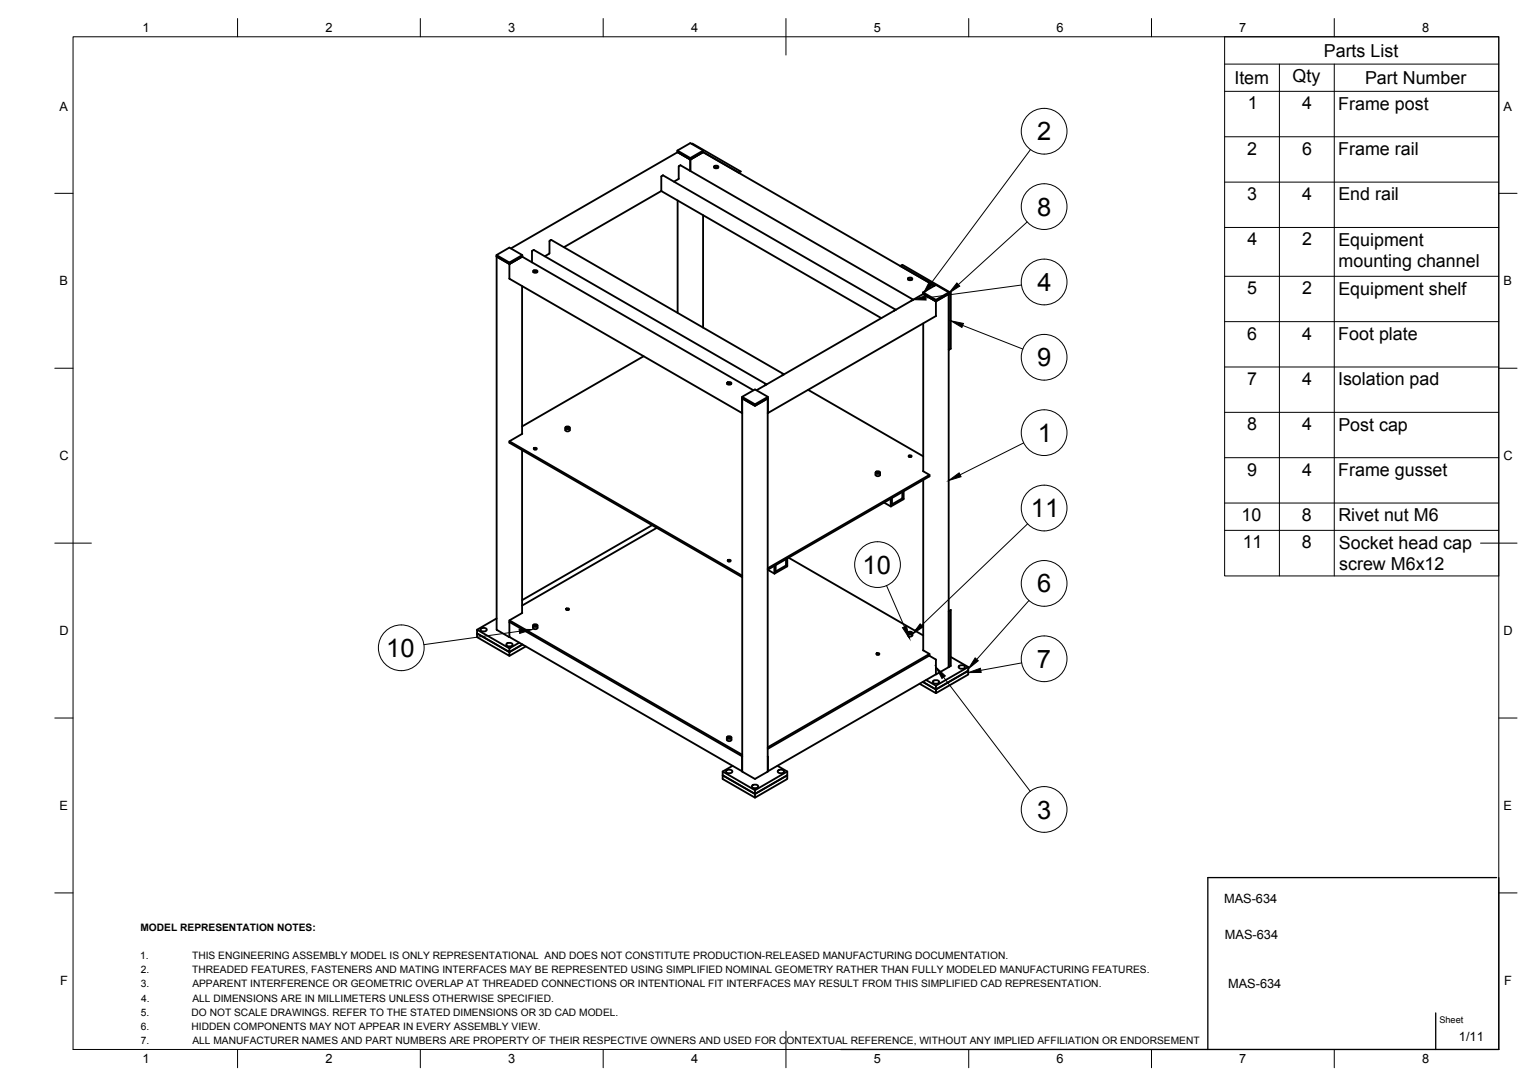
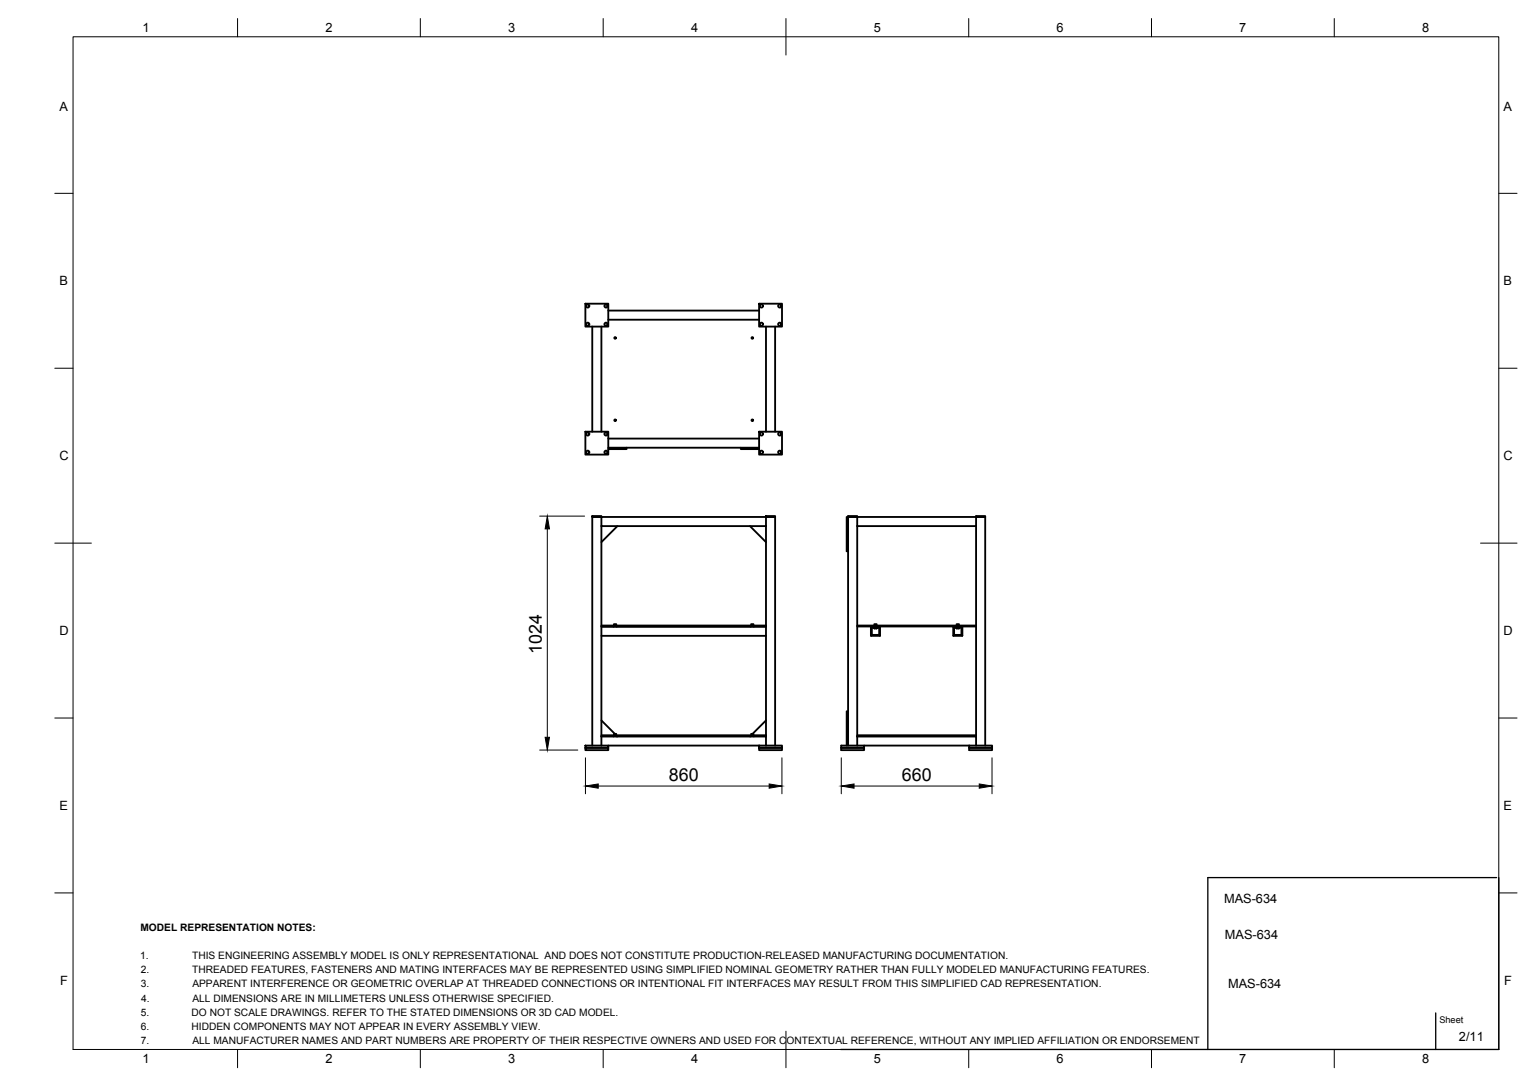
ISO-10303-21;
HEADER;
/* Generated by software containing ST-Developer
 * from STEP Tools, Inc. (www.steptools.com) 
 */

FILE_DESCRIPTION(
/* description */ ('Independent AHU equipment rack. Nominal800x600 frame on1000long40squa
re aluminum posts; two removable notched shelves; welded perimeter/cro
ss rails and rear gussets; two mounting channels; four isolation pads 
and anchor-ready feet. Imported native extrusion library retained and 
cut-length parameters customized per family. Shelf hardware uses model
ed M6 rivet nuts and screws. Weld design, floor anchors and load ratin
g require engineering selection.'),
/* implementation_level */ '2;1');

FILE_NAME(
/* name */ 'MAS-634.step',
/* time_stamp */ '2026-11-07T19:04:45-08:00',
/* author */ (''),
/* organization */ (''),
/* preprocessor_version */ 'ST-DEVELOPER v20.2',
/* originating_system */ 'Autodesk Translation Framework v15.17.0.0',
/* authorisation */ '');

FILE_SCHEMA (('AUTOMOTIVE_DESIGN { 1 0 10303 214 3 1 1 }'));
ENDSEC;

DATA;
#10=MECHANICAL_DESIGN_GEOMETRIC_PRESENTATION_REPRESENTATION('',(#335,#336,
#337,#338,#339,#340,#341,#342,#343,#344,#345),#9777);
#11=ITEM_DEFINED_TRANSFORMATION($,$,#3974,#4302);
#12=ITEM_DEFINED_TRANSFORMATION($,$,#4009,#4303);
#13=ITEM_DEFINED_TRANSFORMATION($,$,#3974,#4304);
#14=ITEM_DEFINED_TRANSFORMATION($,$,#3974,#4305);
#15=ITEM_DEFINED_TRANSFORMATION($,$,#3974,#4306);
#16=ITEM_DEFINED_TRANSFORMATION($,$,#4050,#4307);
#17=ITEM_DEFINED_TRANSFORMATION($,$,#4009,#4308);
#18=ITEM_DEFINED_TRANSFORMATION($,$,#4009,#4309);
#19=ITEM_DEFINED_TRANSFORMATION($,$,#4009,#4310);
#20=ITEM_DEFINED_TRANSFORMATION($,$,#4009,#4311);
#21=ITEM_DEFINED_TRANSFORMATION($,$,#4009,#4312);
#22=ITEM_DEFINED_TRANSFORMATION($,$,#4085,#4313);
#23=ITEM_DEFINED_TRANSFORMATION($,$,#4050,#4314);
#24=ITEM_DEFINED_TRANSFORMATION($,$,#4050,#4315);
#25=ITEM_DEFINED_TRANSFORMATION($,$,#4050,#4316);
#26=ITEM_DEFINED_TRANSFORMATION($,$,#4126,#4317);
#27=ITEM_DEFINED_TRANSFORMATION($,$,#4165,#4318);
#28=ITEM_DEFINED_TRANSFORMATION($,$,#4184,#4319);
#29=ITEM_DEFINED_TRANSFORMATION($,$,#4203,#4320);
#30=ITEM_DEFINED_TRANSFORMATION($,$,#4210,#4321);
#31=ITEM_DEFINED_TRANSFORMATION($,$,#4216,#4322);
#32=ITEM_DEFINED_TRANSFORMATION($,$,#4258,#4323);
#33=ITEM_DEFINED_TRANSFORMATION($,$,#4085,#4324);
#34=ITEM_DEFINED_TRANSFORMATION($,$,#4126,#4325);
#35=ITEM_DEFINED_TRANSFORMATION($,$,#4165,#4326);
#36=ITEM_DEFINED_TRANSFORMATION($,$,#4165,#4327);
#37=ITEM_DEFINED_TRANSFORMATION($,$,#4165,#4328);
#38=ITEM_DEFINED_TRANSFORMATION($,$,#4184,#4329);
#39=ITEM_DEFINED_TRANSFORMATION($,$,#4184,#4330);
#40=ITEM_DEFINED_TRANSFORMATION($,$,#4184,#4331);
#41=ITEM_DEFINED_TRANSFORMATION($,$,#4203,#4332);
#42=ITEM_DEFINED_TRANSFORMATION($,$,#4203,#4333);
#43=ITEM_DEFINED_TRANSFORMATION($,$,#4203,#4334);
#44=ITEM_DEFINED_TRANSFORMATION($,$,#4210,#4335);
#45=ITEM_DEFINED_TRANSFORMATION($,$,#4210,#4336);
#46=ITEM_DEFINED_TRANSFORMATION($,$,#4210,#4337);
#47=ITEM_DEFINED_TRANSFORMATION($,$,#4216,#4338);
#48=ITEM_DEFINED_TRANSFORMATION($,$,#4216,#4339);
#49=ITEM_DEFINED_TRANSFORMATION($,$,#4216,#4340);
#50=ITEM_DEFINED_TRANSFORMATION($,$,#4216,#4341);
#51=ITEM_DEFINED_TRANSFORMATION($,$,#4216,#4342);
#52=ITEM_DEFINED_TRANSFORMATION($,$,#4216,#4343);
#53=ITEM_DEFINED_TRANSFORMATION($,$,#4216,#4344);
#54=ITEM_DEFINED_TRANSFORMATION($,$,#4258,#4345);
#55=ITEM_DEFINED_TRANSFORMATION($,$,#4258,#4346);
#56=ITEM_DEFINED_TRANSFORMATION($,$,#4258,#4347);
#57=ITEM_DEFINED_TRANSFORMATION($,$,#4258,#4348);
#58=ITEM_DEFINED_TRANSFORMATION($,$,#4258,#4349);
#59=ITEM_DEFINED_TRANSFORMATION($,$,#4258,#4350);
#60=ITEM_DEFINED_TRANSFORMATION($,$,#4258,#4351);
#61=(
REPRESENTATION_RELATIONSHIP($,$,#9857,#9856)
REPRESENTATION_RELATIONSHIP_WITH_TRANSFORMATION(#11)
SHAPE_REPRESENTATION_RELATIONSHIP()
);
#62=(
REPRESENTATION_RELATIONSHIP($,$,#9858,#9856)
REPRESENTATION_RELATIONSHIP_WITH_TRANSFORMATION(#12)
SHAPE_REPRESENTATION_RELATIONSHIP()
);
#63=(
REPRESENTATION_RELATIONSHIP($,$,#9857,#9856)
REPRESENTATION_RELATIONSHIP_WITH_TRANSFORMATION(#13)
SHAPE_REPRESENTATION_RELATIONSHIP()
);
#64=(
REPRESENTATION_RELATIONSHIP($,$,#9857,#9856)
REPRESENTATION_RELATIONSHIP_WITH_TRANSFORMATION(#14)
SHAPE_REPRESENTATION_RELATIONSHIP()
);
#65=(
REPRESENTATION_RELATIONSHIP($,$,#9857,#9856)
REPRESENTATION_RELATIONSHIP_WITH_TRANSFORMATION(#15)
SHAPE_REPRESENTATION_RELATIONSHIP()
);
#66=(
REPRESENTATION_RELATIONSHIP($,$,#9859,#9856)
REPRESENTATION_RELATIONSHIP_WITH_TRANSFORMATION(#16)
SHAPE_REPRESENTATION_RELATIONSHIP()
);
#67=(
REPRESENTATION_RELATIONSHIP($,$,#9858,#9856)
REPRESENTATION_RELATIONSHIP_WITH_TRANSFORMATION(#17)
SHAPE_REPRESENTATION_RELATIONSHIP()
);
#68=(
REPRESENTATION_RELATIONSHIP($,$,#9858,#9856)
REPRESENTATION_RELATIONSHIP_WITH_TRANSFORMATION(#18)
SHAPE_REPRESENTATION_RELATIONSHIP()
);
#69=(
REPRESENTATION_RELATIONSHIP($,$,#9858,#9856)
REPRESENTATION_RELATIONSHIP_WITH_TRANSFORMATION(#19)
SHAPE_REPRESENTATION_RELATIONSHIP()
);
#70=(
REPRESENTATION_RELATIONSHIP($,$,#9858,#9856)
REPRESENTATION_RELATIONSHIP_WITH_TRANSFORMATION(#20)
SHAPE_REPRESENTATION_RELATIONSHIP()
);
#71=(
REPRESENTATION_RELATIONSHIP($,$,#9858,#9856)
REPRESENTATION_RELATIONSHIP_WITH_TRANSFORMATION(#21)
SHAPE_REPRESENTATION_RELATIONSHIP()
);
#72=(
REPRESENTATION_RELATIONSHIP($,$,#9860,#9856)
REPRESENTATION_RELATIONSHIP_WITH_TRANSFORMATION(#22)
SHAPE_REPRESENTATION_RELATIONSHIP()
);
#73=(
REPRESENTATION_RELATIONSHIP($,$,#9859,#9856)
REPRESENTATION_RELATIONSHIP_WITH_TRANSFORMATION(#23)
SHAPE_REPRESENTATION_RELATIONSHIP()
);
#74=(
REPRESENTATION_RELATIONSHIP($,$,#9859,#9856)
REPRESENTATION_RELATIONSHIP_WITH_TRANSFORMATION(#24)
SHAPE_REPRESENTATION_RELATIONSHIP()
);
#75=(
REPRESENTATION_RELATIONSHIP($,$,#9859,#9856)
REPRESENTATION_RELATIONSHIP_WITH_TRANSFORMATION(#25)
SHAPE_REPRESENTATION_RELATIONSHIP()
);
#76=(
REPRESENTATION_RELATIONSHIP($,$,#9861,#9856)
REPRESENTATION_RELATIONSHIP_WITH_TRANSFORMATION(#26)
SHAPE_REPRESENTATION_RELATIONSHIP()
);
#77=(
REPRESENTATION_RELATIONSHIP($,$,#9862,#9856)
REPRESENTATION_RELATIONSHIP_WITH_TRANSFORMATION(#27)
SHAPE_REPRESENTATION_RELATIONSHIP()
);
#78=(
REPRESENTATION_RELATIONSHIP($,$,#9863,#9856)
REPRESENTATION_RELATIONSHIP_WITH_TRANSFORMATION(#28)
SHAPE_REPRESENTATION_RELATIONSHIP()
);
#79=(
REPRESENTATION_RELATIONSHIP($,$,#9864,#9856)
REPRESENTATION_RELATIONSHIP_WITH_TRANSFORMATION(#29)
SHAPE_REPRESENTATION_RELATIONSHIP()
);
#80=(
REPRESENTATION_RELATIONSHIP($,$,#9865,#9856)
REPRESENTATION_RELATIONSHIP_WITH_TRANSFORMATION(#30)
SHAPE_REPRESENTATION_RELATIONSHIP()
);
#81=(
REPRESENTATION_RELATIONSHIP($,$,#9866,#9856)
REPRESENTATION_RELATIONSHIP_WITH_TRANSFORMATION(#31)
SHAPE_REPRESENTATION_RELATIONSHIP()
);
#82=(
REPRESENTATION_RELATIONSHIP($,$,#9867,#9856)
REPRESENTATION_RELATIONSHIP_WITH_TRANSFORMATION(#32)
SHAPE_REPRESENTATION_RELATIONSHIP()
);
#83=(
REPRESENTATION_RELATIONSHIP($,$,#9860,#9856)
REPRESENTATION_RELATIONSHIP_WITH_TRANSFORMATION(#33)
SHAPE_REPRESENTATION_RELATIONSHIP()
);
#84=(
REPRESENTATION_RELATIONSHIP($,$,#9861,#9856)
REPRESENTATION_RELATIONSHIP_WITH_TRANSFORMATION(#34)
SHAPE_REPRESENTATION_RELATIONSHIP()
);
#85=(
REPRESENTATION_RELATIONSHIP($,$,#9862,#9856)
REPRESENTATION_RELATIONSHIP_WITH_TRANSFORMATION(#35)
SHAPE_REPRESENTATION_RELATIONSHIP()
);
#86=(
REPRESENTATION_RELATIONSHIP($,$,#9862,#9856)
REPRESENTATION_RELATIONSHIP_WITH_TRANSFORMATION(#36)
SHAPE_REPRESENTATION_RELATIONSHIP()
);
#87=(
REPRESENTATION_RELATIONSHIP($,$,#9862,#9856)
REPRESENTATION_RELATIONSHIP_WITH_TRANSFORMATION(#37)
SHAPE_REPRESENTATION_RELATIONSHIP()
);
#88=(
REPRESENTATION_RELATIONSHIP($,$,#9863,#9856)
REPRESENTATION_RELATIONSHIP_WITH_TRANSFORMATION(#38)
SHAPE_REPRESENTATION_RELATIONSHIP()
);
#89=(
REPRESENTATION_RELATIONSHIP($,$,#9863,#9856)
REPRESENTATION_RELATIONSHIP_WITH_TRANSFORMATION(#39)
SHAPE_REPRESENTATION_RELATIONSHIP()
);
#90=(
REPRESENTATION_RELATIONSHIP($,$,#9863,#9856)
REPRESENTATION_RELATIONSHIP_WITH_TRANSFORMATION(#40)
SHAPE_REPRESENTATION_RELATIONSHIP()
);
#91=(
REPRESENTATION_RELATIONSHIP($,$,#9864,#9856)
REPRESENTATION_RELATIONSHIP_WITH_TRANSFORMATION(#41)
SHAPE_REPRESENTATION_RELATIONSHIP()
);
#92=(
REPRESENTATION_RELATIONSHIP($,$,#9864,#9856)
REPRESENTATION_RELATIONSHIP_WITH_TRANSFORMATION(#42)
SHAPE_REPRESENTATION_RELATIONSHIP()
);
#93=(
REPRESENTATION_RELATIONSHIP($,$,#9864,#9856)
REPRESENTATION_RELATIONSHIP_WITH_TRANSFORMATION(#43)
SHAPE_REPRESENTATION_RELATIONSHIP()
);
#94=(
REPRESENTATION_RELATIONSHIP($,$,#9865,#9856)
REPRESENTATION_RELATIONSHIP_WITH_TRANSFORMATION(#44)
SHAPE_REPRESENTATION_RELATIONSHIP()
);
#95=(
REPRESENTATION_RELATIONSHIP($,$,#9865,#9856)
REPRESENTATION_RELATIONSHIP_WITH_TRANSFORMATION(#45)
SHAPE_REPRESENTATION_RELATIONSHIP()
);
#96=(
REPRESENTATION_RELATIONSHIP($,$,#9865,#9856)
REPRESENTATION_RELATIONSHIP_WITH_TRANSFORMATION(#46)
SHAPE_REPRESENTATION_RELATIONSHIP()
);
#97=(
REPRESENTATION_RELATIONSHIP($,$,#9866,#9856)
REPRESENTATION_RELATIONSHIP_WITH_TRANSFORMATION(#47)
SHAPE_REPRESENTATION_RELATIONSHIP()
);
#98=(
REPRESENTATION_RELATIONSHIP($,$,#9866,#9856)
REPRESENTATION_RELATIONSHIP_WITH_TRANSFORMATION(#48)
SHAPE_REPRESENTATION_RELATIONSHIP()
);
#99=(
REPRESENTATION_RELATIONSHIP($,$,#9866,#9856)
REPRESENTATION_RELATIONSHIP_WITH_TRANSFORMATION(#49)
SHAPE_REPRESENTATION_RELATIONSHIP()
);
#100=(
REPRESENTATION_RELATIONSHIP($,$,#9866,#9856)
REPRESENTATION_RELATIONSHIP_WITH_TRANSFORMATION(#50)
SHAPE_REPRESENTATION_RELATIONSHIP()
);
#101=(
REPRESENTATION_RELATIONSHIP($,$,#9866,#9856)
REPRESENTATION_RELATIONSHIP_WITH_TRANSFORMATION(#51)
SHAPE_REPRESENTATION_RELATIONSHIP()
);
#102=(
REPRESENTATION_RELATIONSHIP($,$,#9866,#9856)
REPRESENTATION_RELATIONSHIP_WITH_TRANSFORMATION(#52)
SHAPE_REPRESENTATION_RELATIONSHIP()
);
#103=(
REPRESENTATION_RELATIONSHIP($,$,#9866,#9856)
REPRESENTATION_RELATIONSHIP_WITH_TRANSFORMATION(#53)
SHAPE_REPRESENTATION_RELATIONSHIP()
);
#104=(
REPRESENTATION_RELATIONSHIP($,$,#9867,#9856)
REPRESENTATION_RELATIONSHIP_WITH_TRANSFORMATION(#54)
SHAPE_REPRESENTATION_RELATIONSHIP()
);
#105=(
REPRESENTATION_RELATIONSHIP($,$,#9867,#9856)
REPRESENTATION_RELATIONSHIP_WITH_TRANSFORMATION(#55)
SHAPE_REPRESENTATION_RELATIONSHIP()
);
#106=(
REPRESENTATION_RELATIONSHIP($,$,#9867,#9856)
REPRESENTATION_RELATIONSHIP_WITH_TRANSFORMATION(#56)
SHAPE_REPRESENTATION_RELATIONSHIP()
);
#107=(
REPRESENTATION_RELATIONSHIP($,$,#9867,#9856)
REPRESENTATION_RELATIONSHIP_WITH_TRANSFORMATION(#57)
SHAPE_REPRESENTATION_RELATIONSHIP()
);
#108=(
REPRESENTATION_RELATIONSHIP($,$,#9867,#9856)
REPRESENTATION_RELATIONSHIP_WITH_TRANSFORMATION(#58)
SHAPE_REPRESENTATION_RELATIONSHIP()
);
#109=(
REPRESENTATION_RELATIONSHIP($,$,#9867,#9856)
REPRESENTATION_RELATIONSHIP_WITH_TRANSFORMATION(#59)
SHAPE_REPRESENTATION_RELATIONSHIP()
);
#110=(
REPRESENTATION_RELATIONSHIP($,$,#9867,#9856)
REPRESENTATION_RELATIONSHIP_WITH_TRANSFORMATION(#60)
SHAPE_REPRESENTATION_RELATIONSHIP()
);
#111=CONTEXT_DEPENDENT_SHAPE_REPRESENTATION(#61,#9806);
#112=CONTEXT_DEPENDENT_SHAPE_REPRESENTATION(#62,#9807);
#113=CONTEXT_DEPENDENT_SHAPE_REPRESENTATION(#63,#9808);
#114=CONTEXT_DEPENDENT_SHAPE_REPRESENTATION(#64,#9809);
#115=CONTEXT_DEPENDENT_SHAPE_REPRESENTATION(#65,#9810);
#116=CONTEXT_DEPENDENT_SHAPE_REPRESENTATION(#66,#9811);
#117=CONTEXT_DEPENDENT_SHAPE_REPRESENTATION(#67,#9812);
#118=CONTEXT_DEPENDENT_SHAPE_REPRESENTATION(#68,#9813);
#119=CONTEXT_DEPENDENT_SHAPE_REPRESENTATION(#69,#9814);
#120=CONTEXT_DEPENDENT_SHAPE_REPRESENTATION(#70,#9815);
#121=CONTEXT_DEPENDENT_SHAPE_REPRESENTATION(#71,#9816);
#122=CONTEXT_DEPENDENT_SHAPE_REPRESENTATION(#72,#9817);
#123=CONTEXT_DEPENDENT_SHAPE_REPRESENTATION(#73,#9818);
#124=CONTEXT_DEPENDENT_SHAPE_REPRESENTATION(#74,#9819);
#125=CONTEXT_DEPENDENT_SHAPE_REPRESENTATION(#75,#9820);
#126=CONTEXT_DEPENDENT_SHAPE_REPRESENTATION(#76,#9821);
#127=CONTEXT_DEPENDENT_SHAPE_REPRESENTATION(#77,#9822);
#128=CONTEXT_DEPENDENT_SHAPE_REPRESENTATION(#78,#9823);
#129=CONTEXT_DEPENDENT_SHAPE_REPRESENTATION(#79,#9824);
#130=CONTEXT_DEPENDENT_SHAPE_REPRESENTATION(#80,#9825);
#131=CONTEXT_DEPENDENT_SHAPE_REPRESENTATION(#81,#9826);
#132=CONTEXT_DEPENDENT_SHAPE_REPRESENTATION(#82,#9827);
#133=CONTEXT_DEPENDENT_SHAPE_REPRESENTATION(#83,#9828);
#134=CONTEXT_DEPENDENT_SHAPE_REPRESENTATION(#84,#9829);
#135=CONTEXT_DEPENDENT_SHAPE_REPRESENTATION(#85,#9830);
#136=CONTEXT_DEPENDENT_SHAPE_REPRESENTATION(#86,#9831);
#137=CONTEXT_DEPENDENT_SHAPE_REPRESENTATION(#87,#9832);
#138=CONTEXT_DEPENDENT_SHAPE_REPRESENTATION(#88,#9833);
#139=CONTEXT_DEPENDENT_SHAPE_REPRESENTATION(#89,#9834);
#140=CONTEXT_DEPENDENT_SHAPE_REPRESENTATION(#90,#9835);
#141=CONTEXT_DEPENDENT_SHAPE_REPRESENTATION(#91,#9836);
#142=CONTEXT_DEPENDENT_SHAPE_REPRESENTATION(#92,#9837);
#143=CONTEXT_DEPENDENT_SHAPE_REPRESENTATION(#93,#9838);
#144=CONTEXT_DEPENDENT_SHAPE_REPRESENTATION(#94,#9839);
#145=CONTEXT_DEPENDENT_SHAPE_REPRESENTATION(#95,#9840);
#146=CONTEXT_DEPENDENT_SHAPE_REPRESENTATION(#96,#9841);
#147=CONTEXT_DEPENDENT_SHAPE_REPRESENTATION(#97,#9842);
#148=CONTEXT_DEPENDENT_SHAPE_REPRESENTATION(#98,#9843);
#149=CONTEXT_DEPENDENT_SHAPE_REPRESENTATION(#99,#9844);
#150=CONTEXT_DEPENDENT_SHAPE_REPRESENTATION(#100,#9845);
#151=CONTEXT_DEPENDENT_SHAPE_REPRESENTATION(#101,#9846);
#152=CONTEXT_DEPENDENT_SHAPE_REPRESENTATION(#102,#9847);
#153=CONTEXT_DEPENDENT_SHAPE_REPRESENTATION(#103,#9848);
#154=CONTEXT_DEPENDENT_SHAPE_REPRESENTATION(#104,#9849);
#155=CONTEXT_DEPENDENT_SHAPE_REPRESENTATION(#105,#9850);
#156=CONTEXT_DEPENDENT_SHAPE_REPRESENTATION(#106,#9851);
#157=CONTEXT_DEPENDENT_SHAPE_REPRESENTATION(#107,#9852);
#158=CONTEXT_DEPENDENT_SHAPE_REPRESENTATION(#108,#9853);
#159=CONTEXT_DEPENDENT_SHAPE_REPRESENTATION(#109,#9854);
#160=CONTEXT_DEPENDENT_SHAPE_REPRESENTATION(#110,#9855);
#161=NEXT_ASSEMBLY_USAGE_OCCURRENCE('Frame post:1','Frame post:1',
'Frame post:1',#9869,#9870,'Frame post:1');
#162=NEXT_ASSEMBLY_USAGE_OCCURRENCE('Frame rail:1','Frame rail:1',
'Frame rail:1',#9869,#9871,'Frame rail:1');
#163=NEXT_ASSEMBLY_USAGE_OCCURRENCE('Frame post:2','Frame post:2',
'Frame post:2',#9869,#9870,'Frame post:2');
#164=NEXT_ASSEMBLY_USAGE_OCCURRENCE('Frame post:3','Frame post:3',
'Frame post:3',#9869,#9870,'Frame post:3');
#165=NEXT_ASSEMBLY_USAGE_OCCURRENCE('Frame post:4','Frame post:4',
'Frame post:4',#9869,#9870,'Frame post:4');
#166=NEXT_ASSEMBLY_USAGE_OCCURRENCE('End rail:1','End rail:1',
'End rail:1',#9869,#9872,'End rail:1');
#167=NEXT_ASSEMBLY_USAGE_OCCURRENCE('Frame rail:2','Frame rail:2',
'Frame rail:2',#9869,#9871,'Frame rail:2');
#168=NEXT_ASSEMBLY_USAGE_OCCURRENCE('Frame rail:3','Frame rail:3',
'Frame rail:3',#9869,#9871,'Frame rail:3');
#169=NEXT_ASSEMBLY_USAGE_OCCURRENCE('Frame rail:4','Frame rail:4',
'Frame rail:4',#9869,#9871,'Frame rail:4');
#170=NEXT_ASSEMBLY_USAGE_OCCURRENCE('Frame rail:5','Frame rail:5',
'Frame rail:5',#9869,#9871,'Frame rail:5');
#171=NEXT_ASSEMBLY_USAGE_OCCURRENCE('Frame rail:6','Frame rail:6',
'Frame rail:6',#9869,#9871,'Frame rail:6');
#172=NEXT_ASSEMBLY_USAGE_OCCURRENCE('Equipment mounting channel:1',
'Equipment mounting channel:1','Equipment mounting channel:1',#9869,#9873,
'Equipment mounting channel:1');
#173=NEXT_ASSEMBLY_USAGE_OCCURRENCE('End rail:2','End rail:2',
'End rail:2',#9869,#9872,'End rail:2');
#174=NEXT_ASSEMBLY_USAGE_OCCURRENCE('End rail:3','End rail:3',
'End rail:3',#9869,#9872,'End rail:3');
#175=NEXT_ASSEMBLY_USAGE_OCCURRENCE('End rail:4','End rail:4',
'End rail:4',#9869,#9872,'End rail:4');
#176=NEXT_ASSEMBLY_USAGE_OCCURRENCE('Equipment shelf:1',
'Equipment shelf:1','Equipment shelf:1',#9869,#9874,'Equipment shelf:1');
#177=NEXT_ASSEMBLY_USAGE_OCCURRENCE('Foot plate:1','Foot plate:1',
'Foot plate:1',#9869,#9875,'Foot plate:1');
#178=NEXT_ASSEMBLY_USAGE_OCCURRENCE('Isolation pad:1','Isolation pad:1',
'Isolation pad:1',#9869,#9876,'Isolation pad:1');
#179=NEXT_ASSEMBLY_USAGE_OCCURRENCE('Post cap:1','Post cap:1',
'Post cap:1',#9869,#9877,'Post cap:1');
#180=NEXT_ASSEMBLY_USAGE_OCCURRENCE('Frame gusset:1','Frame gusset:1',
'Frame gusset:1',#9869,#9878,'Frame gusset:1');
#181=NEXT_ASSEMBLY_USAGE_OCCURRENCE('Rivet nut M6:1','Rivet nut M6:1',
'Rivet nut M6:1',#9869,#9879,'Rivet nut M6:1');
#182=NEXT_ASSEMBLY_USAGE_OCCURRENCE('Socket head cap screw M6x12:1',
'Socket head cap screw M6x12:1','Socket head cap screw M6x12:1',#9869,#9880,
'Socket head cap screw M6x12:1');
#183=NEXT_ASSEMBLY_USAGE_OCCURRENCE('Equipment mounting channel:2',
'Equipment mounting channel:2','Equipment mounting channel:2',#9869,#9873,
'Equipment mounting channel:2');
#184=NEXT_ASSEMBLY_USAGE_OCCURRENCE('Equipment shelf:2',
'Equipment shelf:2','Equipment shelf:2',#9869,#9874,'Equipment shelf:2');
#185=NEXT_ASSEMBLY_USAGE_OCCURRENCE('Foot plate:2','Foot plate:2',
'Foot plate:2',#9869,#9875,'Foot plate:2');
#186=NEXT_ASSEMBLY_USAGE_OCCURRENCE('Foot plate:3','Foot plate:3',
'Foot plate:3',#9869,#9875,'Foot plate:3');
#187=NEXT_ASSEMBLY_USAGE_OCCURRENCE('Foot plate:4','Foot plate:4',
'Foot plate:4',#9869,#9875,'Foot plate:4');
#188=NEXT_ASSEMBLY_USAGE_OCCURRENCE('Isolation pad:2','Isolation pad:2',
'Isolation pad:2',#9869,#9876,'Isolation pad:2');
#189=NEXT_ASSEMBLY_USAGE_OCCURRENCE('Isolation pad:3','Isolation pad:3',
'Isolation pad:3',#9869,#9876,'Isolation pad:3');
#190=NEXT_ASSEMBLY_USAGE_OCCURRENCE('Isolation pad:4','Isolation pad:4',
'Isolation pad:4',#9869,#9876,'Isolation pad:4');
#191=NEXT_ASSEMBLY_USAGE_OCCURRENCE('Post cap:2','Post cap:2',
'Post cap:2',#9869,#9877,'Post cap:2');
#192=NEXT_ASSEMBLY_USAGE_OCCURRENCE('Post cap:3','Post cap:3',
'Post cap:3',#9869,#9877,'Post cap:3');
#193=NEXT_ASSEMBLY_USAGE_OCCURRENCE('Post cap:4','Post cap:4',
'Post cap:4',#9869,#9877,'Post cap:4');
#194=NEXT_ASSEMBLY_USAGE_OCCURRENCE('Frame gusset:2','Frame gusset:2',
'Frame gusset:2',#9869,#9878,'Frame gusset:2');
#195=NEXT_ASSEMBLY_USAGE_OCCURRENCE('Frame gusset:3','Frame gusset:3',
'Frame gusset:3',#9869,#9878,'Frame gusset:3');
#196=NEXT_ASSEMBLY_USAGE_OCCURRENCE('Frame gusset:4','Frame gusset:4',
'Frame gusset:4',#9869,#9878,'Frame gusset:4');
#197=NEXT_ASSEMBLY_USAGE_OCCURRENCE('Rivet nut M6:2','Rivet nut M6:2',
'Rivet nut M6:2',#9869,#9879,'Rivet nut M6:2');
#198=NEXT_ASSEMBLY_USAGE_OCCURRENCE('Rivet nut M6:3','Rivet nut M6:3',
'Rivet nut M6:3',#9869,#9879,'Rivet nut M6:3');
#199=NEXT_ASSEMBLY_USAGE_OCCURRENCE('Rivet nut M6:4','Rivet nut M6:4',
'Rivet nut M6:4',#9869,#9879,'Rivet nut M6:4');
#200=NEXT_ASSEMBLY_USAGE_OCCURRENCE('Rivet nut M6:5','Rivet nut M6:5',
'Rivet nut M6:5',#9869,#9879,'Rivet nut M6:5');
#201=NEXT_ASSEMBLY_USAGE_OCCURRENCE('Rivet nut M6:6','Rivet nut M6:6',
'Rivet nut M6:6',#9869,#9879,'Rivet nut M6:6');
#202=NEXT_ASSEMBLY_USAGE_OCCURRENCE('Rivet nut M6:7','Rivet nut M6:7',
'Rivet nut M6:7',#9869,#9879,'Rivet nut M6:7');
#203=NEXT_ASSEMBLY_USAGE_OCCURRENCE('Rivet nut M6:8','Rivet nut M6:8',
'Rivet nut M6:8',#9869,#9879,'Rivet nut M6:8');
#204=NEXT_ASSEMBLY_USAGE_OCCURRENCE('Socket head cap screw M6x12:2',
'Socket head cap screw M6x12:2','Socket head cap screw M6x12:2',#9869,#9880,
'Socket head cap screw M6x12:2');
#205=NEXT_ASSEMBLY_USAGE_OCCURRENCE('Socket head cap screw M6x12:3',
'Socket head cap screw M6x12:3','Socket head cap screw M6x12:3',#9869,#9880,
'Socket head cap screw M6x12:3');
#206=NEXT_ASSEMBLY_USAGE_OCCURRENCE('Socket head cap screw M6x12:4',
'Socket head cap screw M6x12:4','Socket head cap screw M6x12:4',#9869,#9880,
'Socket head cap screw M6x12:4');
#207=NEXT_ASSEMBLY_USAGE_OCCURRENCE('Socket head cap screw M6x12:5',
'Socket head cap screw M6x12:5','Socket head cap screw M6x12:5',#9869,#9880,
'Socket head cap screw M6x12:5');
#208=NEXT_ASSEMBLY_USAGE_OCCURRENCE('Socket head cap screw M6x12:6',
'Socket head cap screw M6x12:6','Socket head cap screw M6x12:6',#9869,#9880,
'Socket head cap screw M6x12:6');
#209=NEXT_ASSEMBLY_USAGE_OCCURRENCE('Socket head cap screw M6x12:7',
'Socket head cap screw M6x12:7','Socket head cap screw M6x12:7',#9869,#9880,
'Socket head cap screw M6x12:7');
#210=NEXT_ASSEMBLY_USAGE_OCCURRENCE('Socket head cap screw M6x12:8',
'Socket head cap screw M6x12:8','Socket head cap screw M6x12:8',#9869,#9880,
'Socket head cap screw M6x12:8');
#211=CONICAL_SURFACE('',#4283,2.5,0.785398163397449);
#212=B_SPLINE_SURFACE_WITH_KNOTS('',3,3,((#6744,#6745,#6746,#6747,#6748,
#6749,#6750,#6751,#6752,#6753,#6754,#6755,#6756,#6757,#6758,#6759,#6760,
#6761,#6762,#6763,#6764,#6765,#6766,#6767,#6768,#6769,#6770,#6771,#6772,
#6773,#6774,#6775,#6776,#6777,#6778,#6779,#6780,#6781,#6782,#6783,#6784,
#6785,#6786,#6787,#6788,#6789,#6790,#6791,#6792,#6793,#6794,#6795,#6796,
#6797,#6798,#6799,#6800,#6801,#6802,#6803,#6804,#6805),(#6806,#6807,#6808,
#6809,#6810,#6811,#6812,#6813,#6814,#6815,#6816,#6817,#6818,#6819,#6820,
#6821,#6822,#6823,#6824,#6825,#6826,#6827,#6828,#6829,#6830,#6831,#6832,
#6833,#6834,#6835,#6836,#6837,#6838,#6839,#6840,#6841,#6842,#6843,#6844,
#6845,#6846,#6847,#6848,#6849,#6850,#6851,#6852,#6853,#6854,#6855,#6856,
#6857,#6858,#6859,#6860,#6861,#6862,#6863,#6864,#6865,#6866,#6867),(#6868,
#6869,#6870,#6871,#6872,#6873,#6874,#6875,#6876,#6877,#6878,#6879,#6880,
#6881,#6882,#6883,#6884,#6885,#6886,#6887,#6888,#6889,#6890,#6891,#6892,
#6893,#6894,#6895,#6896,#6897,#6898,#6899,#6900,#6901,#6902,#6903,#6904,
#6905,#6906,#6907,#6908,#6909,#6910,#6911,#6912,#6913,#6914,#6915,#6916,
#6917,#6918,#6919,#6920,#6921,#6922,#6923,#6924,#6925,#6926,#6927,#6928,
#6929),(#6930,#6931,#6932,#6933,#6934,#6935,#6936,#6937,#6938,#6939,#6940,
#6941,#6942,#6943,#6944,#6945,#6946,#6947,#6948,#6949,#6950,#6951,#6952,
#6953,#6954,#6955,#6956,#6957,#6958,#6959,#6960,#6961,#6962,#6963,#6964,
#6965,#6966,#6967,#6968,#6969,#6970,#6971,#6972,#6973,#6974,#6975,#6976,
#6977,#6978,#6979,#6980,#6981,#6982,#6983,#6984,#6985,#6986,#6987,#6988,
#6989,#6990,#6991)),.UNSPECIFIED.,.F.,.F.,.F.,(4,4),(4,1,1,1,1,1,1,1,1,
1,1,1,1,1,1,1,1,1,1,1,1,1,1,1,1,1,1,1,1,1,1,1,1,1,1,1,1,1,1,1,1,1,1,1,1,
1,1,1,1,1,1,1,1,1,1,1,1,1,1,4),(0.,0.0642013499338864),(11.8589888623078,
12.8516263649797,13.8442638676517,14.8369013703236,15.8295388729956,16.8221763756675,
17.8148138783394,18.8074513810114,19.8000888836833,20.7927263863553,21.7853638890272,
22.7780013916992,23.7706388943711,24.7632763970431,25.755913899715,26.7485514023869,
27.7411889050589,28.7338264077308,29.7264639104028,30.7191014130747,31.7117389157467,
32.7043764184186,33.6970139210906,34.6896514237625,35.6822889264344,36.6749264291064,
37.6675639317783,38.6602014344503,39.6528389371222,40.6454764397942,41.6381139424661,
42.6307514451381,43.62338894781,44.6160264504819,45.6086639531539,46.6013014558258,
47.5939389584978,48.5865764611697,49.5792139638417,50.5718514665136,51.5644889691856,
52.5571264718575,53.5497639745294,54.5424014772014,55.5350389798733,56.5276764825453,
57.5203139852172,58.5129514878892,59.5055889905611,60.4982264932331,61.490863995905,
62.4835014985769,63.4761390012489,64.4687765039208,65.4614140065928,66.4540515092647,
67.4466890119367,68.4393265146086,69.4319640172805,70.4246015199525),
 .UNSPECIFIED.);
#213=B_SPLINE_SURFACE_WITH_KNOTS('',3,3,((#7196,#7197,#7198,#7199,#7200,
#7201,#7202,#7203,#7204,#7205,#7206,#7207,#7208,#7209,#7210,#7211,#7212,
#7213,#7214,#7215,#7216,#7217,#7218,#7219,#7220,#7221,#7222,#7223,#7224,
#7225,#7226,#7227,#7228,#7229,#7230,#7231,#7232,#7233,#7234,#7235,#7236,
#7237,#7238,#7239,#7240,#7241,#7242,#7243,#7244,#7245,#7246,#7247,#7248,
#7249,#7250,#7251,#7252,#7253,#7254,#7255,#7256,#7257),(#7258,#7259,#7260,
#7261,#7262,#7263,#7264,#7265,#7266,#7267,#7268,#7269,#7270,#7271,#7272,
#7273,#7274,#7275,#7276,#7277,#7278,#7279,#7280,#7281,#7282,#7283,#7284,
#7285,#7286,#7287,#7288,#7289,#7290,#7291,#7292,#7293,#7294,#7295,#7296,
#7297,#7298,#7299,#7300,#7301,#7302,#7303,#7304,#7305,#7306,#7307,#7308,
#7309,#7310,#7311,#7312,#7313,#7314,#7315,#7316,#7317,#7318,#7319),(#7320,
#7321,#7322,#7323,#7324,#7325,#7326,#7327,#7328,#7329,#7330,#7331,#7332,
#7333,#7334,#7335,#7336,#7337,#7338,#7339,#7340,#7341,#7342,#7343,#7344,
#7345,#7346,#7347,#7348,#7349,#7350,#7351,#7352,#7353,#7354,#7355,#7356,
#7357,#7358,#7359,#7360,#7361,#7362,#7363,#7364,#7365,#7366,#7367,#7368,
#7369,#7370,#7371,#7372,#7373,#7374,#7375,#7376,#7377,#7378,#7379,#7380,
#7381),(#7382,#7383,#7384,#7385,#7386,#7387,#7388,#7389,#7390,#7391,#7392,
#7393,#7394,#7395,#7396,#7397,#7398,#7399,#7400,#7401,#7402,#7403,#7404,
#7405,#7406,#7407,#7408,#7409,#7410,#7411,#7412,#7413,#7414,#7415,#7416,
#7417,#7418,#7419,#7420,#7421,#7422,#7423,#7424,#7425,#7426,#7427,#7428,
#7429,#7430,#7431,#7432,#7433,#7434,#7435,#7436,#7437,#7438,#7439,#7440,
#7441,#7442,#7443)),.UNSPECIFIED.,.F.,.F.,.F.,(4,4),(4,1,1,1,1,1,1,1,1,
1,1,1,1,1,1,1,1,1,1,1,1,1,1,1,1,1,1,1,1,1,1,1,1,1,1,1,1,1,1,1,1,1,1,1,1,
1,1,1,1,1,1,1,1,1,1,1,1,1,1,4),(0.,0.0642013499338864),(14.3984001269718,
15.3910376296438,16.3836751323157,17.3763126349876,18.3689501376596,19.3615876403315,
20.3542251430035,21.3468626456754,22.3395001483474,23.3321376510193,24.3247751536913,
25.3174126563632,26.3100501590351,27.3026876617071,28.295325164379,29.287962667051,
30.2806001697229,31.2732376723949,32.2658751750668,33.2585126777388,34.2511501804107,
35.2437876830827,36.2364251857546,37.2290626884265,38.2217001910985,39.2143376937704,
40.2069751964424,41.1996126991143,42.1922502017863,43.1848877044582,44.1775252071302,
45.1701627098021,46.162800212474,47.155437715146,48.1480752178179,49.1407127204899,
50.1333502231618,51.1259877258338,52.1186252285057,53.1112627311777,54.1039002338496,
55.0965377365215,56.0891752391935,57.0818127418654,58.0744502445374,59.0670877472093,
60.0597252498813,61.0523627525532,62.0450002552252,63.0376377578971,64.0302752605691,
65.022912763241,66.0155502659129,67.0081877685849,68.0008252712568,68.9934627739288,
69.9861002766007,70.9787377792727,71.9713752819446,72.9640127846166),
 .UNSPECIFIED.);
#214=B_SPLINE_SURFACE_WITH_KNOTS('',3,3,((#8793,#8794,#8795,#8796,#8797,
#8798,#8799,#8800,#8801,#8802,#8803,#8804,#8805,#8806,#8807,#8808,#8809,
#8810,#8811,#8812,#8813,#8814,#8815,#8816,#8817,#8818,#8819,#8820,#8821,
#8822,#8823,#8824,#8825,#8826,#8827,#8828,#8829,#8830,#8831,#8832,#8833,
#8834,#8835,#8836,#8837,#8838,#8839,#8840,#8841,#8842,#8843,#8844,#8845,
#8846,#8847,#8848,#8849,#8850,#8851,#8852,#8853,#8854,#8855,#8856,#8857,
#8858,#8859,#8860,#8861,#8862,#8863,#8864,#8865,#8866,#8867,#8868,#8869),
(#8870,#8871,#8872,#8873,#8874,#8875,#8876,#8877,#8878,#8879,#8880,#8881,
#8882,#8883,#8884,#8885,#8886,#8887,#8888,#8889,#8890,#8891,#8892,#8893,
#8894,#8895,#8896,#8897,#8898,#8899,#8900,#8901,#8902,#8903,#8904,#8905,
#8906,#8907,#8908,#8909,#8910,#8911,#8912,#8913,#8914,#8915,#8916,#8917,
#8918,#8919,#8920,#8921,#8922,#8923,#8924,#8925,#8926,#8927,#8928,#8929,
#8930,#8931,#8932,#8933,#8934,#8935,#8936,#8937,#8938,#8939,#8940,#8941,
#8942,#8943,#8944,#8945,#8946),(#8947,#8948,#8949,#8950,#8951,#8952,#8953,
#8954,#8955,#8956,#8957,#8958,#8959,#8960,#8961,#8962,#8963,#8964,#8965,
#8966,#8967,#8968,#8969,#8970,#8971,#8972,#8973,#8974,#8975,#8976,#8977,
#8978,#8979,#8980,#8981,#8982,#8983,#8984,#8985,#8986,#8987,#8988,#8989,
#8990,#8991,#8992,#8993,#8994,#8995,#8996,#8997,#8998,#8999,#9000,#9001,
#9002,#9003,#9004,#9005,#9006,#9007,#9008,#9009,#9010,#9011,#9012,#9013,
#9014,#9015,#9016,#9017,#9018,#9019,#9020,#9021,#9022,#9023),(#9024,#9025,
#9026,#9027,#9028,#9029,#9030,#9031,#9032,#9033,#9034,#9035,#9036,#9037,
#9038,#9039,#9040,#9041,#9042,#9043,#9044,#9045,#9046,#9047,#9048,#9049,
#9050,#9051,#9052,#9053,#9054,#9055,#9056,#9057,#9058,#9059,#9060,#9061,
#9062,#9063,#9064,#9065,#9066,#9067,#9068,#9069,#9070,#9071,#9072,#9073,
#9074,#9075,#9076,#9077,#9078,#9079,#9080,#9081,#9082,#9083,#9084,#9085,
#9086,#9087,#9088,#9089,#9090,#9091,#9092,#9093,#9094,#9095,#9096,#9097,
#9098,#9099,#9100)),.UNSPECIFIED.,.F.,.F.,.F.,(4,4),(4,1,1,1,1,1,1,1,1,
1,1,1,1,1,1,1,1,1,1,1,1,1,1,1,1,1,1,1,1,1,1,1,1,1,1,1,1,1,1,1,1,1,1,1,1,
1,1,1,1,1,1,1,1,1,1,1,1,1,1,1,1,1,1,1,1,1,1,1,1,1,1,1,1,1,4),(0.,0.0658467982010768),
(11.6150328478182,12.6023632471184,13.5896936464185,14.5770240457187,15.5643544450188,
16.551684844319,17.5390152436191,18.5263456429193,19.5136760422194,20.5010064415196,
21.4883368408197,22.4756672401199,23.46299763942,24.4503280387202,25.4376584380203,
26.4249888373205,27.4123192366206,28.3996496359208,29.3869800352209,30.3743104345211,
31.3616408338212,32.3489712331214,33.3363016324215,34.3236320317217,35.3109624310218,
36.298292830322,37.2856232296221,38.2729536289223,39.2602840282224,40.2476144275226,
41.2349448268227,42.2222752261229,43.209605625423,44.1969360247232,45.1842664240233,
46.1715968233235,47.1589272226236,48.1462576219238,49.1335880212239,50.1209184205241,
51.1082488198242,52.0955792191244,53.0829096184245,54.0702400177247,55.0575704170248,
56.0449008163249,57.0322312156251,58.0195616149252,59.0068920142254,59.9942224135255,
60.9815528128257,61.9688832121258,62.956213611426,63.9435440107261,64.9308744100263,
65.9182048093264,66.9055352086266,67.8928656079267,68.8801960072269,69.867526406527,
70.8548568058272,71.8421872051273,72.8295176044275,73.8168480037276,74.8041784030278,
75.7915088023279,76.7788392016281,77.7661696009282,78.7535000002284,79.7408303995285,
80.7281607988287,81.7154911981288,82.702821597429,83.6901519967291,84.6774823960293),
 .UNSPECIFIED.);
#215=B_SPLINE_SURFACE_WITH_KNOTS('',3,3,((#9229,#9230,#9231,#9232,#9233,
#9234,#9235,#9236,#9237,#9238,#9239,#9240,#9241,#9242,#9243,#9244,#9245,
#9246,#9247,#9248,#9249,#9250,#9251,#9252,#9253,#9254,#9255,#9256,#9257,
#9258,#9259,#9260,#9261,#9262,#9263,#9264,#9265,#9266,#9267,#9268,#9269,
#9270,#9271,#9272,#9273,#9274,#9275,#9276,#9277,#9278,#9279,#9280,#9281,
#9282,#9283,#9284,#9285,#9286,#9287,#9288,#9289,#9290,#9291,#9292,#9293,
#9294,#9295,#9296,#9297,#9298,#9299,#9300,#9301,#9302,#9303,#9304,#9305,
#9306,#9307),(#9308,#9309,#9310,#9311,#9312,#9313,#9314,#9315,#9316,#9317,
#9318,#9319,#9320,#9321,#9322,#9323,#9324,#9325,#9326,#9327,#9328,#9329,
#9330,#9331,#9332,#9333,#9334,#9335,#9336,#9337,#9338,#9339,#9340,#9341,
#9342,#9343,#9344,#9345,#9346,#9347,#9348,#9349,#9350,#9351,#9352,#9353,
#9354,#9355,#9356,#9357,#9358,#9359,#9360,#9361,#9362,#9363,#9364,#9365,
#9366,#9367,#9368,#9369,#9370,#9371,#9372,#9373,#9374,#9375,#9376,#9377,
#9378,#9379,#9380,#9381,#9382,#9383,#9384,#9385,#9386),(#9387,#9388,#9389,
#9390,#9391,#9392,#9393,#9394,#9395,#9396,#9397,#9398,#9399,#9400,#9401,
#9402,#9403,#9404,#9405,#9406,#9407,#9408,#9409,#9410,#9411,#9412,#9413,
#9414,#9415,#9416,#9417,#9418,#9419,#9420,#9421,#9422,#9423,#9424,#9425,
#9426,#9427,#9428,#9429,#9430,#9431,#9432,#9433,#9434,#9435,#9436,#9437,
#9438,#9439,#9440,#9441,#9442,#9443,#9444,#9445,#9446,#9447,#9448,#9449,
#9450,#9451,#9452,#9453,#9454,#9455,#9456,#9457,#9458,#9459,#9460,#9461,
#9462,#9463,#9464,#9465),(#9466,#9467,#9468,#9469,#9470,#9471,#9472,#9473,
#9474,#9475,#9476,#9477,#9478,#9479,#9480,#9481,#9482,#9483,#9484,#9485,
#9486,#9487,#9488,#9489,#9490,#9491,#9492,#9493,#9494,#9495,#9496,#9497,
#9498,#9499,#9500,#9501,#9502,#9503,#9504,#9505,#9506,#9507,#9508,#9509,
#9510,#9511,#9512,#9513,#9514,#9515,#9516,#9517,#9518,#9519,#9520,#9521,
#9522,#9523,#9524,#9525,#9526,#9527,#9528,#9529,#9530,#9531,#9532,#9533,
#9534,#9535,#9536,#9537,#9538,#9539,#9540,#9541,#9542,#9543,#9544)),
 .UNSPECIFIED.,.F.,.F.,.F.,(4,4),(4,1,1,1,1,1,1,1,1,1,1,1,1,1,1,1,1,1,1,
1,1,1,1,1,1,1,1,1,1,1,1,1,1,1,1,1,1,1,1,1,1,1,1,1,1,1,1,1,1,1,1,1,1,1,1,
1,1,1,1,1,1,1,1,1,1,1,1,1,1,1,1,1,1,1,1,1,4),(0.,0.0658467982010768),(8.30747755240104,
9.2960444961263,10.2846114398516,11.2731783835768,12.2617453273021,13.2503122710274,
14.2388792147526,15.2274461584779,16.2160131022032,17.2045800459284,18.1931469896537,
19.181713933379,20.1702808771042,21.1588478208295,22.1474147645547,23.13598170828,
24.1245486520053,25.1131155957305,26.1016825394558,27.0902494831811,28.0788164269063,
29.0673833706316,30.0559503143569,31.0445172580821,32.0330842018074,33.0216511455327,
34.0102180892579,34.9987850329832,35.9873519767085,36.9759189204337,37.964485864159,
38.9530528078842,39.9416197516095,40.9301866953348,41.91875363906,42.9073205827853,
43.8958875265106,44.8844544702358,45.8730214139611,46.8615883576864,47.8501553014116,
48.8387222451369,49.8272891888622,50.8158561325874,51.8044230763127,52.792990020038,
53.7815569637632,54.7701239074885,55.7586908512138,56.747257794939,57.7358247386643,
58.7243916823895,59.7129586261148,60.7015255698401,61.6900925135653,62.6786594572906,
63.6672264010159,64.6557933447411,65.6443602884664,66.6329272321917,67.6214941759169,
68.6100611196422,69.5986280633675,70.5871950070927,71.575761950818,72.5643288945433,
73.5528958382685,74.5414627819938,75.530029725719,76.5185966694443,77.5071636131696,
78.4957305568948,79.4842975006201,80.4728644443454,81.4614313880706,82.4499983317959,
83.4385652755212),.UNSPECIFIED.);
#216=B_SPLINE_CURVE_WITH_KNOTS('',3,(#6103,#6104,#6105,#6106,#6107,#6108,
#6109,#6110,#6111,#6112,#6113,#6114,#6115),.UNSPECIFIED.,.F.,.F.,(4,3,3,
3,4),(-3.84897440564114,-2.97791250801583,-1.98527500534389,-0.992637502671945,
0.),.UNSPECIFIED.);
#217=B_SPLINE_CURVE_WITH_KNOTS('',3,(#6118,#6119,#6120,#6121,#6122,#6123,
#6124,#6125,#6126,#6127,#6128,#6129,#6130,#6131,#6132,#6133,#6134,#6135,
#6136),.UNSPECIFIED.,.F.,.F.,(4,3,3,3,3,3,4),(2.01694489302846,2.97791250801583,
3.97055001068778,4.96318751335972,5.95582501603167,6.94846251870361,7.59274844815667),
 .UNSPECIFIED.);
#218=B_SPLINE_CURVE_WITH_KNOTS('',3,(#6141,#6142,#6143,#6144,#6145,#6146,
#6147,#6148,#6149,#6150,#6151,#6152,#6153,#6154,#6155,#6156,#6157,#6158,
#6159,#6160,#6161,#6162,#6163,#6164,#6165),.UNSPECIFIED.,.F.,.F.,(4,3,3,
3,3,3,3,3,4),(-10.1321597128207,-9.92637502671944,-8.9337375240475,-7.94110002137556,
-6.94846251870361,-5.95582501603167,-4.96318751335972,-3.97055001068778,
-3.84897440564114),.UNSPECIFIED.);
#219=B_SPLINE_CURVE_WITH_KNOTS('',3,(#6166,#6167,#6168,#6169,#6170,#6171,
#6172,#6173,#6174,#6175,#6176,#6177,#6178,#6179,#6180,#6181,#6182,#6183,
#6184,#6185,#6186,#6187),.UNSPECIFIED.,.F.,.F.,(4,3,3,3,3,3,3,4),(7.59274844815667,
7.94110002137556,8.9337375240475,9.92637502671945,10.9190125293914,11.9116500320633,
12.9042875347353,13.8759337553363),.UNSPECIFIED.);
#220=B_SPLINE_CURVE_WITH_KNOTS('',3,(#6192,#6193,#6194,#6195,#6196,#6197,
#6198,#6199,#6200,#6201,#6202,#6203,#6204,#6205,#6206,#6207,#6208,#6209,
#6210,#6211,#6212,#6213),.UNSPECIFIED.,.F.,.F.,(4,3,3,3,3,3,3,4),(-16.4153450200003,
-15.8822000427511,-14.8895625400792,-13.8969250374072,-12.9042875347353,
-11.9116500320633,-10.9190125293914,-10.1321597128207),.UNSPECIFIED.);
#221=B_SPLINE_CURVE_WITH_KNOTS('',3,(#6214,#6215,#6216,#6217,#6218,#6219,
#6220,#6221,#6222,#6223,#6224,#6225,#6226,#6227,#6228,#6229,#6230,#6231,
#6232,#6233,#6234,#6235,#6236,#6237,#6238),.UNSPECIFIED.,.F.,.F.,(4,3,3,
3,3,3,3,3,4),(13.8759337553363,13.8969250374072,14.8895625400792,15.8822000427511,
16.8748375454231,17.867475048095,18.860112550767,19.8527500534389,20.1591190625158),
 .UNSPECIFIED.);
#222=B_SPLINE_CURVE_WITH_KNOTS('',3,(#6243,#6244,#6245,#6246,#6247,#6248,
#6249,#6250,#6251,#6252,#6253,#6254,#6255,#6256,#6257,#6258,#6259,#6260,
#6261,#6262,#6263,#6264),.UNSPECIFIED.,.F.,.F.,(4,3,3,3,3,3,3,4),(-22.6985303271799,
-21.8380250587828,-20.8453875561108,-19.8527500534389,-18.8601125507669,
-17.867475048095,-16.8748375454231,-16.4153450200003),.UNSPECIFIED.);
#223=B_SPLINE_CURVE_WITH_KNOTS('',3,(#6265,#6266,#6267,#6268,#6269,#6270,
#6271,#6272,#6273,#6274,#6275,#6276,#6277,#6278,#6279,#6280,#6281,#6282,
#6283,#6284,#6285,#6286),.UNSPECIFIED.,.F.,.F.,(4,3,3,3,3,3,3,4),(20.1591190625158,
20.8453875561109,21.8380250587828,22.8306625614547,23.8233000641267,24.8159375667986,
25.8085750694706,26.4423043696954),.UNSPECIFIED.);
#224=B_SPLINE_CURVE_WITH_KNOTS('',3,(#6291,#6292,#6293,#6294,#6295,#6296,
#6297,#6298,#6299,#6300,#6301,#6302,#6303,#6304,#6305,#6306,#6307,#6308,
#6309,#6310,#6311,#6312,#6313,#6314,#6315),.UNSPECIFIED.,.F.,.F.,(4,3,3,
3,3,3,3,3,4),(-28.9817156343595,-28.7864875774864,-27.7938500748144,-26.8012125721425,
-25.8085750694705,-24.8159375667986,-23.8233000641267,-22.8306625614547,
-22.6985303271799),.UNSPECIFIED.);
#225=B_SPLINE_CURVE_WITH_KNOTS('',3,(#6316,#6317,#6318,#6319,#6320,#6321,
#6322,#6323,#6324,#6325,#6326,#6327,#6328,#6329,#6330,#6331,#6332,#6333,
#6334,#6335,#6336,#6337),.UNSPECIFIED.,.F.,.F.,(4,3,3,3,3,3,3,4),(26.4423043696954,
26.8012125721425,27.7938500748145,28.7864875774864,29.7791250801584,30.7717625828303,
31.7644000855022,32.725489676875),.UNSPECIFIED.);
#226=B_SPLINE_CURVE_WITH_KNOTS('',3,(#6342,#6343,#6344,#6345,#6346,#6347,
#6348,#6349,#6350,#6351,#6352,#6353,#6354,#6355,#6356,#6357,#6358,#6359,
#6360,#6361,#6362,#6363),.UNSPECIFIED.,.F.,.F.,(4,3,3,3,3,3,3,4),(-35.2649009415391,
-34.7423125935181,-33.7496750908461,-32.7570375881742,-31.7644000855022,
-30.7717625828303,-29.7791250801583,-28.9817156343595),.UNSPECIFIED.);
#227=B_SPLINE_CURVE_WITH_KNOTS('',3,(#6364,#6365,#6366,#6367,#6368,#6369,
#6370,#6371,#6372,#6373,#6374,#6375,#6376,#6377,#6378,#6379,#6380,#6381,
#6382,#6383,#6384,#6385,#6386,#6387,#6388),.UNSPECIFIED.,.F.,.F.,(4,3,3,
3,3,3,3,3,4),(32.725489676875,32.7570375881742,33.7496750908461,34.7423125935181,
35.73495009619,36.727587598862,37.7202251015339,38.7128626042059,39.0086749840546),
 .UNSPECIFIED.);
#228=B_SPLINE_CURVE_WITH_KNOTS('',3,(#6393,#6394,#6395,#6396,#6397,#6398,
#6399,#6400,#6401,#6402,#6403,#6404,#6405,#6406,#6407,#6408,#6409,#6410,
#6411,#6412,#6413,#6414),.UNSPECIFIED.,.F.,.F.,(4,3,3,3,3,3,3,4),(-41.5480862487187,
-40.6981376095497,-39.7055001068778,-38.7128626042058,-37.7202251015339,
-36.7275875988619,-35.73495009619,-35.2649009415391),.UNSPECIFIED.);
#229=B_SPLINE_CURVE_WITH_KNOTS('',3,(#6415,#6416,#6417,#6418,#6419,#6420,
#6421,#6422,#6423,#6424,#6425,#6426,#6427,#6428,#6429,#6430,#6431,#6432,
#6433,#6434,#6435,#6436),.UNSPECIFIED.,.F.,.F.,(4,3,3,3,3,3,3,4),(39.0086749840546,
39.7055001068778,40.6981376095497,41.6907751122217,42.6834126148936,43.6760501175656,
44.6686876202375,45.2918602912342),.UNSPECIFIED.);
#230=B_SPLINE_CURVE_WITH_KNOTS('',3,(#6441,#6442,#6443,#6444,#6445,#6446,
#6447,#6448,#6449,#6450,#6451,#6452,#6453,#6454,#6455,#6456,#6457,#6458,
#6459,#6460,#6461,#6462,#6463,#6464,#6465),.UNSPECIFIED.,.F.,.F.,(4,3,3,
3,3,3,3,3,4),(-47.8312715558982,-47.6466001282533,-46.6539626255814,-45.6613251229094,
-44.6686876202375,-43.6760501175656,-42.6834126148936,-41.6907751122217,
-41.5480862487187),.UNSPECIFIED.);
#231=B_SPLINE_CURVE_WITH_KNOTS('',3,(#6466,#6467,#6468,#6469,#6470,#6471,
#6472,#6473,#6474,#6475,#6476,#6477,#6478,#6479,#6480,#6481,#6482,#6483,
#6484,#6485,#6486,#6487),.UNSPECIFIED.,.F.,.F.,(4,3,3,3,3,3,3,4),(45.2918602912342,
45.6613251229095,46.6539626255814,47.6466001282534,48.6392376309253,49.6318751335972,
50.6245126362692,51.5750455984138),.UNSPECIFIED.);
#232=B_SPLINE_CURVE_WITH_KNOTS('',3,(#6493,#6494,#6495,#6496),
 .UNSPECIFIED.,.F.,.F.,(4,4),(57.8582309055934,58.5656126576447),
 .UNSPECIFIED.);
#233=B_SPLINE_CURVE_WITH_KNOTS('',3,(#6499,#6500,#6501,#6502,#6503,#6504,
#6505,#6506,#6507,#6508),.UNSPECIFIED.,.F.,.F.,(4,3,3,4),(-56.5486677646163,
-55.5877001496289,-54.5950626469569,-54.1144568630778),.UNSPECIFIED.);
#234=B_SPLINE_CURVE_WITH_KNOTS('',3,(#6514,#6515,#6516,#6517,#6518,#6519,
#6520,#6521),.UNSPECIFIED.,.F.,.F.,(4,1,1,1,1,4),(65.9734457253856,66.4540515092647,
67.4466890119367,68.4393265146086,69.4319640172805,70.4246015199525),
 .UNSPECIFIED.);
#235=B_SPLINE_CURVE_WITH_KNOTS('',3,(#6524,#6525,#6526,#6527,#6528,#6529,
#6530,#6531,#6532),.UNSPECIFIED.,.F.,.F.,(4,1,1,1,1,1,4),(65.9734457253856,
66.0155502659129,67.0081877685849,68.0008252712568,68.9934627739288,69.9861002766007,
70.9470678915881),.UNSPECIFIED.);
#236=B_SPLINE_CURVE_WITH_KNOTS('',3,(#6537,#6538,#6539,#6540,#6541,#6542,
#6543,#6544,#6545,#6546),.UNSPECIFIED.,.F.,.F.,(4,1,1,1,1,1,1,4),(59.6902604182061,
60.4982264932331,61.490863995905,62.4835014985769,63.4761390012489,64.4687765039208,
65.4614140065928,65.9734457253856),.UNSPECIFIED.);
#237=B_SPLINE_CURVE_WITH_KNOTS('',3,(#6547,#6548,#6549,#6550,#6551,#6552,
#6553,#6554,#6555,#6556),.UNSPECIFIED.,.F.,.F.,(4,1,1,1,1,1,1,4),(59.6902604182061,
60.0597252498813,61.0523627525532,62.0450002552252,63.0376377578971,64.0302752605691,
65.022912763241,65.9734457253856),.UNSPECIFIED.);
#238=B_SPLINE_CURVE_WITH_KNOTS('',3,(#6561,#6562,#6563,#6564,#6565,#6566,
#6567,#6568,#6569,#6570,#6571),.UNSPECIFIED.,.F.,.F.,(4,1,1,1,1,1,1,1,4),
(53.4070751110265,53.5497639745294,54.5424014772014,55.5350389798733,56.5276764825453,
57.5203139852172,58.5129514878892,59.5055889905611,59.6902604182061),
 .UNSPECIFIED.);
#239=B_SPLINE_CURVE_WITH_KNOTS('',3,(#6572,#6573,#6574,#6575,#6576,#6577,
#6578,#6579,#6580,#6581),.UNSPECIFIED.,.F.,.F.,(4,1,1,1,1,1,1,4),(53.4070751110265,
54.1039002338496,55.0965377365215,56.0891752391935,57.0818127418654,58.0744502445374,
59.0670877472093,59.6902604182061),.UNSPECIFIED.);
#240=B_SPLINE_CURVE_WITH_KNOTS('',3,(#6586,#6587,#6588,#6589,#6590,#6591,
#6592,#6593,#6594,#6595),.UNSPECIFIED.,.F.,.F.,(4,1,1,1,1,1,1,4),(47.1238898038469,
47.5939389584978,48.5865764611697,49.5792139638417,50.5718514665136,51.5644889691856,
52.5571264718575,53.4070751110265),.UNSPECIFIED.);
#241=B_SPLINE_CURVE_WITH_KNOTS('',3,(#6596,#6597,#6598,#6599,#6600,#6601,
#6602,#6603,#6604,#6605,#6606),.UNSPECIFIED.,.F.,.F.,(4,1,1,1,1,1,1,1,4),
(47.1238898038469,47.155437715146,48.1480752178179,49.1407127204899,50.1333502231618,
51.1259877258338,52.1186252285057,53.1112627311777,53.4070751110265),
 .UNSPECIFIED.);
#242=B_SPLINE_CURVE_WITH_KNOTS('',3,(#6611,#6612,#6613,#6614,#6615,#6616,
#6617,#6618,#6619,#6620),.UNSPECIFIED.,.F.,.F.,(4,1,1,1,1,1,1,4),(40.8407044966673,
41.6381139424661,42.6307514451381,43.62338894781,44.6160264504819,45.6086639531539,
46.6013014558258,47.1238898038469),.UNSPECIFIED.);
#243=B_SPLINE_CURVE_WITH_KNOTS('',3,(#6621,#6622,#6623,#6624,#6625,#6626,
#6627,#6628,#6629,#6630),.UNSPECIFIED.,.F.,.F.,(4,1,1,1,1,1,1,4),(40.8407044966673,
41.1996126991143,42.1922502017863,43.1848877044582,44.1775252071302,45.1701627098021,
46.162800212474,47.1238898038469),.UNSPECIFIED.);
#244=B_SPLINE_CURVE_WITH_KNOTS('',3,(#6635,#6636,#6637,#6638,#6639,#6640,
#6641,#6642,#6643,#6644,#6645),.UNSPECIFIED.,.F.,.F.,(4,1,1,1,1,1,1,1,4),
(34.5575191894877,34.6896514237625,35.6822889264344,36.6749264291064,37.6675639317783,
38.6602014344503,39.6528389371222,40.6454764397942,40.8407044966673),
 .UNSPECIFIED.);
#245=B_SPLINE_CURVE_WITH_KNOTS('',3,(#6646,#6647,#6648,#6649,#6650,#6651,
#6652,#6653,#6654,#6655),.UNSPECIFIED.,.F.,.F.,(4,1,1,1,1,1,1,4),(34.5575191894877,
35.2437876830827,36.2364251857546,37.2290626884265,38.2217001910985,39.2143376937704,
40.2069751964424,40.8407044966673),.UNSPECIFIED.);
#246=B_SPLINE_CURVE_WITH_KNOTS('',3,(#6660,#6661,#6662,#6663,#6664,#6665,
#6666,#6667,#6668,#6669),.UNSPECIFIED.,.F.,.F.,(4,1,1,1,1,1,1,4),(28.2743338823081,
28.7338264077308,29.7264639104028,30.7191014130747,31.7117389157467,32.7043764184186,
33.6970139210906,34.5575191894877),.UNSPECIFIED.);
#247=B_SPLINE_CURVE_WITH_KNOTS('',3,(#6670,#6671,#6672,#6673,#6674,#6675,
#6676,#6677,#6678,#6679,#6680),.UNSPECIFIED.,.F.,.F.,(4,1,1,1,1,1,1,1,4),
(28.2743338823081,28.295325164379,29.287962667051,30.2806001697229,31.2732376723949,
32.2658751750668,33.2585126777388,34.2511501804107,34.5575191894877),
 .UNSPECIFIED.);
#248=B_SPLINE_CURVE_WITH_KNOTS('',3,(#6685,#6686,#6687,#6688,#6689,#6690,
#6691,#6692,#6693,#6694),.UNSPECIFIED.,.F.,.F.,(4,1,1,1,1,1,1,4),(21.9911485751285,
22.7780013916992,23.7706388943711,24.7632763970431,25.755913899715,26.7485514023869,
27.7411889050589,28.2743338823081),.UNSPECIFIED.);
#249=B_SPLINE_CURVE_WITH_KNOTS('',3,(#6695,#6696,#6697,#6698,#6699,#6700,
#6701,#6702,#6703,#6704),.UNSPECIFIED.,.F.,.F.,(4,1,1,1,1,1,1,4),(21.9911485751285,
22.3395001483474,23.3321376510193,24.3247751536913,25.3174126563632,26.3100501590351,
27.3026876617071,28.2743338823081),.UNSPECIFIED.);
#250=B_SPLINE_CURVE_WITH_KNOTS('',3,(#6710,#6711,#6712,#6713,#6714),
 .UNSPECIFIED.,.F.,.F.,(4,1,4),(14.3984001269718,15.3910376296438,15.7079632679489),
 .UNSPECIFIED.);
#251=B_SPLINE_CURVE_WITH_KNOTS('',3,(#6717,#6718,#6719,#6720,#6721),
 .UNSPECIFIED.,.F.,.F.,(4,1,4),(13.8759337553362,14.8369013703236,15.7079632679489),
 .UNSPECIFIED.);
#252=B_SPLINE_CURVE_WITH_KNOTS('',3,(#6723,#6724,#6725,#6726,#6727,#6728,
#6729,#6730,#6731,#6732,#6733),.UNSPECIFIED.,.F.,.F.,(4,1,1,1,1,1,1,1,4),
(15.7079632679489,15.8295388729956,16.8221763756675,17.8148138783394,18.8074513810114,
19.8000888836833,20.7927263863553,21.7853638890272,21.9911485751285),
 .UNSPECIFIED.);
#253=B_SPLINE_CURVE_WITH_KNOTS('',3,(#6734,#6735,#6736,#6737,#6738,#6739,
#6740,#6741,#6742,#6743),.UNSPECIFIED.,.F.,.F.,(4,1,1,1,1,1,1,4),(15.7079632679489,
16.3836751323157,17.3763126349876,18.3689501376596,19.3615876403315,20.3542251430035,
21.3468626456754,21.9911485751285),.UNSPECIFIED.);
#254=B_SPLINE_CURVE_WITH_KNOTS('',3,(#6992,#6993,#6994,#6995,#6996,#6997,
#6998,#6999,#7000,#7001,#7002,#7003,#7004,#7005,#7006,#7007,#7008,#7009,
#7010,#7011,#7012,#7013,#7014,#7015,#7016,#7017,#7018,#7019,#7020,#7021,
#7022,#7023,#7024,#7025,#7026,#7027,#7028,#7029,#7030,#7031,#7032,#7033,
#7034,#7035,#7036,#7037,#7038,#7039,#7040,#7041,#7042,#7043,#7044,#7045,
#7046,#7047,#7048,#7049,#7050,#7051,#7052,#7053,#7054,#7055,#7056,#7057,
#7058,#7059,#7060,#7061,#7062,#7063,#7064,#7065,#7066,#7067,#7068,#7069,
#7070,#7071,#7072,#7073,#7074,#7075,#7076,#7077,#7078,#7079,#7080,#7081,
#7082),.UNSPECIFIED.,.F.,.F.,(4,3,3,3,3,3,3,3,3,3,3,3,3,3,3,3,3,3,3,3,3,
3,3,3,3,3,3,3,3,3,4),(0.,0.0297334041407413,0.060121188705027,0.0893594248720358,
0.114942881518169,0.12062818802643,0.150387503639245,0.17998043773465,0.208492097811262,
0.220468872654926,0.228874065707467,0.234174696232567,0.264100887136832,
0.292003393472183,0.294027078041098,0.3229737914971,0.339361239182251,0.343534194645605,
0.371627921656661,0.399766246005302,0.427498548100254,0.437962627154652,
0.445613074679864,0.450368652920306,0.478071944275567,0.498849412792013,
0.508237562401581,0.513366228472013,0.539276359085418,0.561181818341351,
0.569248610399392),.UNSPECIFIED.);
#255=B_SPLINE_CURVE_WITH_KNOTS('',3,(#7083,#7084,#7085,#7086,#7087,#7088,
#7089,#7090,#7091,#7092,#7093,#7094,#7095,#7096,#7097,#7098,#7099,#7100,
#7101,#7102,#7103,#7104,#7105,#7106,#7107,#7108,#7109,#7110,#7111,#7112,
#7113,#7114,#7115,#7116,#7117,#7118,#7119,#7120,#7121,#7122,#7123,#7124,
#7125,#7126,#7127,#7128,#7129,#7130,#7131,#7132,#7133,#7134,#7135,#7136,
#7137,#7138,#7139,#7140,#7141,#7142,#7143,#7144,#7145,#7146,#7147,#7148,
#7149,#7150,#7151,#7152,#7153,#7154,#7155,#7156,#7157,#7158,#7159,#7160,
#7161,#7162,#7163,#7164,#7165,#7166,#7167,#7168,#7169,#7170,#7171,#7172,
#7173),.UNSPECIFIED.,.F.,.F.,(4,3,3,3,3,3,3,3,3,3,3,3,3,3,3,3,3,3,3,3,3,
3,3,3,3,3,3,3,3,3,4),(0.,0.0253741918154253,0.0514188574543204,0.0781724584567371,
0.0899216140471938,0.0966260843074363,0.102679517247254,0.129987895141776,
0.157743514226617,0.184669552038376,0.1959299763122,0.202971688416046,0.207100127397784,
0.236273896435719,0.265447665473654,0.293335582735069,0.30266718021653,
0.30870328948035,0.314529473155204,0.342600363170572,0.371717504292952,
0.401165116978085,0.421327065973589,0.426436909350868,0.456483211929156,
0.481642425143559,0.494284407148645,0.499857105743045,0.530355157019413,
0.557120064786768,0.566847306048084),.UNSPECIFIED.);
#256=B_SPLINE_CURVE_WITH_KNOTS('',3,(#7174,#7175,#7176,#7177,#7178,#7179,
#7180,#7181,#7182,#7183,#7184,#7185,#7186,#7187,#7188,#7189,#7190,#7191,
#7192,#7193,#7194,#7195),.UNSPECIFIED.,.F.,.F.,(4,3,3,3,3,3,3,4),(-54.1144568630778,
-53.602425144285,-52.609787641613,-51.6171501389411,-50.6245126362692,-49.6318751335972,
-48.6392376309253,-47.8312715558982),.UNSPECIFIED.);
#257=B_SPLINE_CURVE_WITH_KNOTS('',3,(#7444,#7445,#7446,#7447,#7448,#7449,
#7450,#7451,#7452,#7453,#7454,#7455,#7456,#7457,#7458,#7459,#7460,#7461,
#7462,#7463,#7464,#7465,#7466,#7467,#7468,#7469,#7470,#7471,#7472,#7473,
#7474,#7475,#7476,#7477,#7478,#7479,#7480,#7481,#7482,#7483,#7484,#7485,
#7486,#7487,#7488,#7489,#7490,#7491,#7492,#7493,#7494,#7495,#7496,#7497,
#7498,#7499,#7500,#7501,#7502,#7503,#7504,#7505,#7506,#7507,#7508,#7509,
#7510,#7511,#7512,#7513,#7514,#7515,#7516,#7517,#7518,#7519,#7520,#7521,
#7522,#7523,#7524,#7525,#7526,#7527,#7528,#7529,#7530,#7531,#7532,#7533,
#7534),.UNSPECIFIED.,.F.,.F.,(4,3,3,3,3,3,3,3,3,3,3,3,3,3,3,3,3,3,3,3,3,
3,3,3,3,3,3,3,3,3,4),(0.,0.0253741449502821,0.0514187685629996,0.0781723806768318,
0.0899215962667811,0.0966260820429981,0.10267951725872,0.129987863111654,
0.157743467348106,0.184669516879494,0.195929969047891,0.202971685861533,
0.207100122286109,0.236273893879883,0.265447665473657,0.293335606992279,
0.302667231074582,0.30870349429627,0.314529468018238,0.342600392862402,
0.371717549581951,0.401165166107868,0.421327178828175,0.42643689855922,
0.456483208176513,0.481642422329078,0.494284406072129,0.499857109233687,
0.530355160772762,0.557120064786773,0.566847306048096),.UNSPECIFIED.);
#258=B_SPLINE_CURVE_WITH_KNOTS('',3,(#7535,#7536,#7537,#7538,#7539,#7540,
#7541,#7542,#7543,#7544,#7545,#7546,#7547,#7548,#7549,#7550,#7551,#7552,
#7553,#7554,#7555,#7556,#7557,#7558,#7559),.UNSPECIFIED.,.F.,.F.,(4,3,3,
3,3,3,3,3,4),(51.5750455984138,51.6171501389411,52.6097876416131,53.602425144285,
54.595062646957,55.5877001496289,56.5803376523009,57.5729751549728,57.8582309055934),
 .UNSPECIFIED.);
#259=B_SPLINE_CURVE_WITH_KNOTS('',3,(#7560,#7561,#7562,#7563,#7564,#7565,
#7566,#7567,#7568,#7569,#7570,#7571,#7572,#7573,#7574,#7575,#7576,#7577,
#7578,#7579,#7580,#7581,#7582,#7583,#7584,#7585,#7586,#7587,#7588,#7589,
#7590,#7591,#7592,#7593,#7594,#7595,#7596,#7597,#7598,#7599,#7600,#7601,
#7602,#7603,#7604,#7605,#7606,#7607,#7608,#7609,#7610,#7611,#7612,#7613,
#7614,#7615,#7616,#7617,#7618,#7619,#7620,#7621,#7622,#7623,#7624,#7625,
#7626,#7627,#7628,#7629,#7630,#7631,#7632,#7633,#7634,#7635,#7636,#7637,
#7638,#7639,#7640,#7641,#7642,#7643,#7644,#7645,#7646,#7647,#7648,#7649,
#7650),.UNSPECIFIED.,.F.,.F.,(4,3,3,3,3,3,3,3,3,3,3,3,3,3,3,3,3,3,3,3,3,
3,3,3,3,3,3,3,3,3,4),(0.,0.0297333652245644,0.0601211311135188,0.0893593744794667,
0.114942837424671,0.120628184894895,0.150387501019274,0.179980446751773,
0.208492104574105,0.220468888246807,0.228874110566872,0.234174709732106,
0.264100893886604,0.292003410907553,0.294027078041101,0.322973790194836,
0.339361247095814,0.343534203933017,0.371627930217731,0.399766255738478,
0.427498569351598,0.437962674970173,0.44561323665522,0.450368688624651,
0.478071971053836,0.498849432875724,0.508237633125922,0.51336624635807,
0.539276402540273,0.561181818341388,0.569248610399427),.UNSPECIFIED.);
#260=B_SPLINE_CURVE_WITH_KNOTS('',3,(#7687,#7688,#7689,#7690,#7691,#7692,
#7693,#7694,#7695,#7696),.UNSPECIFIED.,.F.,.F.,(4,3,3,4),(-4.09293042013066,
-3.9493215972006,-2.96199119790045,-2.06863817490914),.UNSPECIFIED.);
#261=B_SPLINE_CURVE_WITH_KNOTS('',3,(#7699,#7700,#7701,#7702,#7703,#7704,
#7705),.UNSPECIFIED.,.F.,.F.,(4,3,4),(0.,0.988566943725272,1.11730040836823),
 .UNSPECIFIED.);
#262=B_SPLINE_CURVE_WITH_KNOTS('',3,(#7710,#7711,#7712,#7713,#7714,#7715,
#7716,#7717,#7718,#7719,#7720,#7721,#7722,#7723,#7724,#7725,#7726,#7727,
#7728,#7729,#7730,#7731),.UNSPECIFIED.,.F.,.F.,(4,3,3,3,3,3,3,4),(-10.3761157273102,
-9.87330399300149,-8.88597359370134,-7.89864319440119,-6.91131279510104,
-5.92398239580089,-4.93665199650074,-4.09293042013066),.UNSPECIFIED.);
#263=B_SPLINE_CURVE_WITH_KNOTS('',3,(#7732,#7733,#7734,#7735,#7736,#7737,
#7738,#7739,#7740,#7741,#7742,#7743,#7744,#7745,#7746,#7747,#7748,#7749,
#7750,#7751,#7752,#7753),.UNSPECIFIED.,.F.,.F.,(4,3,3,3,3,3,3,4),(1.11730040836823,
1.97713388745054,2.9657008311758,3.95426777490106,4.94283471862632,5.93140166235159,
6.91996860607685,7.40048571554782),.UNSPECIFIED.);
#264=B_SPLINE_CURVE_WITH_KNOTS('',3,(#7758,#7759,#7760,#7761,#7762,#7763,
#7764,#7765,#7766,#7767,#7768,#7769,#7770,#7771,#7772,#7773,#7774,#7775,
#7776,#7777,#7778,#7779),.UNSPECIFIED.,.F.,.F.,(4,3,3,3,3,3,3,4),(-16.6593010344898,
-15.7972863888024,-14.8099559895022,-13.8226255902021,-12.8352951909019,
-11.8479647916018,-10.8606343923016,-10.3761157273102),.UNSPECIFIED.);
#265=B_SPLINE_CURVE_WITH_KNOTS('',3,(#7780,#7781,#7782,#7783,#7784,#7785,
#7786,#7787,#7788,#7789,#7790,#7791,#7792,#7793,#7794,#7795,#7796,#7797,
#7798,#7799,#7800,#7801),.UNSPECIFIED.,.F.,.F.,(4,3,3,3,3,3,3,4),(7.40048571554782,
7.90853554980211,8.89710249352738,9.88566943725264,10.8742363809779,11.8628033247032,
12.8513702684284,13.6836710227274),.UNSPECIFIED.);
#266=B_SPLINE_CURVE_WITH_KNOTS('',3,(#7806,#7807,#7808,#7809,#7810,#7811,
#7812,#7813,#7814,#7815,#7816,#7817,#7818,#7819,#7820,#7821,#7822,#7823,
#7824,#7825,#7826,#7827,#7828,#7829,#7830),.UNSPECIFIED.,.F.,.F.,(4,3,3,
3,3,3,3,3,4),(-22.9424863416694,-22.7085991839034,-21.7212687846033,-20.7339383853031,
-19.746607986003,-18.7592775867028,-17.7719471874027,-16.7846167881025,
-16.6593010344898),.UNSPECIFIED.);
#267=B_SPLINE_CURVE_WITH_KNOTS('',3,(#7831,#7832,#7833,#7834,#7835,#7836,
#7837,#7838,#7839,#7840,#7841,#7842,#7843,#7844,#7845,#7846,#7847,#7848,
#7849,#7850,#7851,#7852,#7853,#7854,#7855),.UNSPECIFIED.,.F.,.F.,(4,3,3,
3,3,3,3,3,4),(13.6836710227274,13.8399372121537,14.828504155879,15.8170710996042,
16.8056380433295,17.7942049870548,18.78277193078,19.7713388745053,19.966856329907),
 .UNSPECIFIED.);
#268=B_SPLINE_CURVE_WITH_KNOTS('',3,(#7860,#7861,#7862,#7863,#7864,#7865,
#7866,#7867,#7868,#7869,#7870,#7871,#7872,#7873,#7874,#7875,#7876,#7877,
#7878,#7879,#7880,#7881),.UNSPECIFIED.,.F.,.F.,(4,3,3,3,3,3,3,4),(-29.225671648849,
-28.6325815797043,-27.6452511804042,-26.657920781104,-25.6705903818039,
-24.6832599825037,-23.6959295832036,-22.9424863416694),.UNSPECIFIED.);
#269=B_SPLINE_CURVE_WITH_KNOTS('',3,(#7882,#7883,#7884,#7885,#7886,#7887,
#7888,#7889,#7890,#7891,#7892,#7893,#7894,#7895,#7896,#7897,#7898,#7899,
#7900,#7901,#7902,#7903),.UNSPECIFIED.,.F.,.F.,(4,3,3,3,3,3,3,4),(19.966856329907,
20.7599058182306,21.7484727619558,22.7370397056811,23.7256066494064,24.7141735931316,
25.7027405368569,26.2500416370866),.UNSPECIFIED.);
#270=B_SPLINE_CURVE_WITH_KNOTS('',3,(#7908,#7909,#7910,#7911,#7912,#7913,
#7914,#7915,#7916,#7917,#7918,#7919,#7920,#7921,#7922,#7923,#7924,#7925,
#7926,#7927,#7928,#7929),.UNSPECIFIED.,.F.,.F.,(4,3,3,3,3,3,3,4),(-35.5088569560286,
-34.5565639755052,-33.5692335762051,-32.5819031769049,-31.5945727776048,
-30.6072423783046,-29.6199119790045,-29.225671648849),.UNSPECIFIED.);
#271=B_SPLINE_CURVE_WITH_KNOTS('',3,(#7930,#7931,#7932,#7933,#7934,#7935,
#7936,#7937,#7938,#7939,#7940,#7941,#7942,#7943,#7944,#7945,#7946,#7947,
#7948,#7949,#7950,#7951),.UNSPECIFIED.,.F.,.F.,(4,3,3,3,3,3,3,4),(26.2500416370866,
26.6913074805822,27.6798744243074,28.6684413680327,29.6570083117579,30.6455752554832,
31.6341421992085,32.5332269442662),.UNSPECIFIED.);
#272=B_SPLINE_CURVE_WITH_KNOTS('',3,(#7956,#7957,#7958,#7959,#7960,#7961,
#7962,#7963,#7964,#7965,#7966,#7967,#7968,#7969,#7970,#7971,#7972,#7973,
#7974,#7975,#7976,#7977,#7978,#7979,#7980),.UNSPECIFIED.,.F.,.F.,(4,3,3,
3,3,3,3,3,4),(-41.7920422632082,-41.4678767706063,-40.4805463713061,-39.4932159720059,
-38.5058855727058,-37.5185551734057,-36.5312247741055,-35.5438943748054,
-35.5088569560286),.UNSPECIFIED.);
#273=B_SPLINE_CURVE_WITH_KNOTS('',3,(#7981,#7982,#7983,#7984,#7985,#7986,
#7987,#7988,#7989,#7990,#7991,#7992,#7993,#7994,#7995,#7996,#7997,#7998,
#7999,#8000,#8001,#8002,#8003,#8004,#8005),.UNSPECIFIED.,.F.,.F.,(4,3,3,
3,3,3,3,3,4),(32.5332269442662,32.6227091429337,33.611276086659,34.5998430303843,
35.5884099741095,36.5769769178348,37.5655438615601,38.5541108052853,38.8164122514458),
 .UNSPECIFIED.);
#274=B_SPLINE_CURVE_WITH_KNOTS('',3,(#8010,#8011,#8012,#8013,#8014,#8015,
#8016,#8017,#8018,#8019,#8020,#8021,#8022,#8023,#8024,#8025,#8026,#8027,
#8028,#8029,#8030,#8031),.UNSPECIFIED.,.F.,.F.,(4,3,3,3,3,3,3,4),(-48.0752275703878,
-47.3918591664071,-46.404528767107,-45.4171983678069,-44.4298679685067,
-43.4425375692066,-42.4552071699064,-41.7920422632082),.UNSPECIFIED.);
#275=B_SPLINE_CURVE_WITH_KNOTS('',3,(#8032,#8033,#8034,#8035,#8036,#8037,
#8038,#8039,#8040,#8041,#8042,#8043,#8044,#8045,#8046,#8047,#8048,#8049,
#8050,#8051,#8052,#8053),.UNSPECIFIED.,.F.,.F.,(4,3,3,3,3,3,3,4),(38.8164122514458,
39.5426777490106,40.5312446927359,41.5198116364611,42.5083785801864,43.4969455239117,
44.4855124676369,45.0995975586253),.UNSPECIFIED.);
#276=B_SPLINE_CURVE_WITH_KNOTS('',3,(#8058,#8059,#8060,#8061,#8062,#8063,
#8064,#8065,#8066,#8067,#8068,#8069,#8070,#8071,#8072,#8073,#8074,#8075,
#8076,#8077,#8078,#8079,#8080,#8081,#8082),.UNSPECIFIED.,.F.,.F.,(4,3,3,
3,3,3,3,3,4),(-54.3584128775674,-54.3031719615082,-53.315841562208,-52.3285111629079,
-51.3411807636077,-50.3538503643076,-49.3665199650074,-48.3791895657073,
-48.0752275703878),.UNSPECIFIED.);
#277=B_SPLINE_CURVE_WITH_KNOTS('',3,(#8083,#8084,#8085,#8086,#8087,#8088,
#8089,#8090,#8091,#8092,#8093,#8094,#8095,#8096,#8097,#8098,#8099,#8100,
#8101,#8102,#8103,#8104),.UNSPECIFIED.,.F.,.F.,(4,3,3,3,3,3,3,4),(45.0995975586253,
45.4740794113622,46.4626463550875,47.4512132988127,48.439780242538,49.4283471862633,
50.4169141299885,51.3827828658049),.UNSPECIFIED.);
#278=B_SPLINE_CURVE_WITH_KNOTS('',3,(#8109,#8110,#8111,#8112,#8113,#8114,
#8115,#8116,#8117,#8118,#8119,#8120,#8121,#8122,#8123,#8124,#8125,#8126,
#8127,#8128,#8129,#8130),.UNSPECIFIED.,.F.,.F.,(4,3,3,3,3,3,3,4),(-60.641598184747,
-60.2271543573091,-59.2398239580089,-58.2524935587088,-57.2651631594086,
-56.2778327601085,-55.2905023608083,-54.3584128775674),.UNSPECIFIED.);
#279=B_SPLINE_CURVE_WITH_KNOTS('',3,(#8131,#8132,#8133,#8134,#8135,#8136,
#8137,#8138,#8139,#8140,#8141,#8142,#8143,#8144,#8145,#8146,#8147,#8148,
#8149,#8150,#8151,#8152,#8153,#8154,#8155),.UNSPECIFIED.,.F.,.F.,(4,3,3,
3,3,3,3,3,4),(51.3827828658049,51.4054810737138,52.394048017439,53.3826149611643,
54.3711819048896,55.3597488486148,56.3483157923401,57.3368827360654,57.6659681729845),
 .UNSPECIFIED.);
#280=B_SPLINE_CURVE_WITH_KNOTS('',3,(#8160,#8161,#8162,#8163,#8164,#8165,
#8166,#8167,#8168,#8169,#8170,#8171,#8172,#8173,#8174,#8175,#8176,#8177,
#8178,#8179,#8180,#8181),.UNSPECIFIED.,.F.,.F.,(4,3,3,3,3,3,3,4),(-66.9247834919266,
-66.15113675311,-65.1638063538098,-64.1764759545097,-63.1891455552095,-62.2018151559094,
-61.2144847566092,-60.641598184747),.UNSPECIFIED.);
#281=B_SPLINE_CURVE_WITH_KNOTS('',3,(#8182,#8183,#8184,#8185,#8186,#8187,
#8188,#8189,#8190,#8191,#8192,#8193,#8194,#8195,#8196,#8197,#8198,#8199,
#8200,#8201,#8202,#8203),.UNSPECIFIED.,.F.,.F.,(4,3,3,3,3,3,3,4),(57.6659681729845,
58.3254496797906,59.3140166235159,60.3025835672412,61.2911505109664,62.2797174546917,
63.268284398417,63.9491534801641),.UNSPECIFIED.);
#282=B_SPLINE_CURVE_WITH_KNOTS('',3,(#8209,#8210,#8211,#8212,#8213,#8214,
#8215,#8216,#8217,#8218),.UNSPECIFIED.,.F.,.F.,(4,1,1,1,1,1,1,4),(78.5398163397448,
78.7535000002284,79.7408303995285,80.7281607988287,81.7154911981288,82.702821597429,
83.6901519967291,84.6774823960293),.UNSPECIFIED.);
#283=B_SPLINE_CURVE_WITH_KNOTS('',3,(#8221,#8222,#8223,#8224,#8225,#8226,
#8227,#8228),.UNSPECIFIED.,.F.,.F.,(4,1,1,1,1,4),(78.5398163397448,79.4842975006201,
80.4728644443454,81.4614313880706,82.4499983317959,83.4385652755212),
 .UNSPECIFIED.);
#284=B_SPLINE_CURVE_WITH_KNOTS('',3,(#8233,#8234,#8235,#8236,#8237,#8238,
#8239,#8240,#8241,#8242),.UNSPECIFIED.,.F.,.F.,(4,1,1,1,1,1,1,4),(72.2566310325653,
72.8295176044275,73.8168480037276,74.8041784030278,75.7915088023279,76.7788392016281,
77.7661696009282,78.5398163397448),.UNSPECIFIED.);
#285=B_SPLINE_CURVE_WITH_KNOTS('',3,(#8243,#8244,#8245,#8246,#8247,#8248,
#8249,#8250,#8251,#8252,#8253),.UNSPECIFIED.,.F.,.F.,(4,1,1,1,1,1,1,1,4),
(72.2566310325652,72.5643288945433,73.5528958382685,74.5414627819938,75.530029725719,
76.5185966694443,77.5071636131696,78.4957305568948,78.5398163397448),
 .UNSPECIFIED.);
#286=B_SPLINE_CURVE_WITH_KNOTS('',3,(#8258,#8259,#8260,#8261,#8262,#8263,
#8264,#8265,#8266,#8267),.UNSPECIFIED.,.F.,.F.,(4,1,1,1,1,1,1,4),(65.9734457253856,
66.9055352086266,67.8928656079267,68.8801960072269,69.867526406527,70.8548568058272,
71.8421872051273,72.2566310325653),.UNSPECIFIED.);
#287=B_SPLINE_CURVE_WITH_KNOTS('',3,(#8268,#8269,#8270,#8271,#8272,#8273,
#8274,#8275,#8276,#8277),.UNSPECIFIED.,.F.,.F.,(4,1,1,1,1,1,1,4),(65.9734457253856,
66.6329272321917,67.6214941759169,68.6100611196422,69.5986280633675,70.5871950070927,
71.575761950818,72.2566310325652),.UNSPECIFIED.);
#288=B_SPLINE_CURVE_WITH_KNOTS('',3,(#8282,#8283,#8284,#8285,#8286,#8287,
#8288,#8289,#8290,#8291,#8292),.UNSPECIFIED.,.F.,.F.,(4,1,1,1,1,1,1,1,4),
(59.6902604182061,59.9942224135255,60.9815528128257,61.9688832121258,62.956213611426,
63.9435440107261,64.9308744100263,65.9182048093264,65.9734457253856),
 .UNSPECIFIED.);
#289=B_SPLINE_CURVE_WITH_KNOTS('',3,(#8293,#8294,#8295,#8296,#8297,#8298,
#8299,#8300,#8301,#8302,#8303),.UNSPECIFIED.,.F.,.F.,(4,1,1,1,1,1,1,1,4),
(59.6902604182061,59.7129586261148,60.7015255698401,61.6900925135653,62.6786594572906,
63.6672264010159,64.6557933447411,65.6443602884664,65.9734457253856),
 .UNSPECIFIED.);
#290=B_SPLINE_CURVE_WITH_KNOTS('',3,(#8308,#8309,#8310,#8311,#8312,#8313,
#8314,#8315,#8316,#8317),.UNSPECIFIED.,.F.,.F.,(4,1,1,1,1,1,1,4),(53.4070751110265,
54.0702400177247,55.0575704170248,56.0449008163249,57.0322312156251,58.0195616149252,
59.0068920142254,59.6902604182061),.UNSPECIFIED.);
#291=B_SPLINE_CURVE_WITH_KNOTS('',3,(#8318,#8319,#8320,#8321,#8322,#8323,
#8324,#8325,#8326,#8327),.UNSPECIFIED.,.F.,.F.,(4,1,1,1,1,1,1,4),(53.4070751110265,
53.7815569637632,54.7701239074885,55.7586908512138,56.747257794939,57.7358247386643,
58.7243916823895,59.6902604182061),.UNSPECIFIED.);
#292=B_SPLINE_CURVE_WITH_KNOTS('',3,(#8332,#8333,#8334,#8335,#8336,#8337,
#8338,#8339,#8340,#8341,#8342),.UNSPECIFIED.,.F.,.F.,(4,1,1,1,1,1,1,1,4),
(47.1238898038469,47.1589272226236,48.1462576219238,49.1335880212239,50.1209184205241,
51.1082488198242,52.0955792191244,53.0829096184245,53.4070751110265),
 .UNSPECIFIED.);
#293=B_SPLINE_CURVE_WITH_KNOTS('',3,(#8343,#8344,#8345,#8346,#8347,#8348,
#8349,#8350,#8351,#8352),.UNSPECIFIED.,.F.,.F.,(4,1,1,1,1,1,1,4),(47.1238898038469,
47.8501553014116,48.8387222451369,49.8272891888622,50.8158561325874,51.8044230763127,
52.792990020038,53.4070751110265),.UNSPECIFIED.);
#294=B_SPLINE_CURVE_WITH_KNOTS('',3,(#8357,#8358,#8359,#8360,#8361,#8362,
#8363,#8364,#8365,#8366),.UNSPECIFIED.,.F.,.F.,(4,1,1,1,1,1,1,4),(40.8407044966673,
41.2349448268227,42.2222752261229,43.209605625423,44.1969360247232,45.1842664240233,
46.1715968233235,47.1238898038469),.UNSPECIFIED.);
#295=B_SPLINE_CURVE_WITH_KNOTS('',3,(#8367,#8368,#8369,#8370,#8371,#8372,
#8373,#8374,#8375,#8376,#8377),.UNSPECIFIED.,.F.,.F.,(4,1,1,1,1,1,1,1,4),
(40.8407044966673,40.9301866953348,41.91875363906,42.9073205827853,43.8958875265106,
44.8844544702358,45.8730214139611,46.8615883576864,47.1238898038469),
 .UNSPECIFIED.);
#296=B_SPLINE_CURVE_WITH_KNOTS('',3,(#8382,#8383,#8384,#8385,#8386,#8387,
#8388,#8389,#8390,#8391),.UNSPECIFIED.,.F.,.F.,(4,1,1,1,1,1,1,4),(34.5575191894877,
35.3109624310218,36.298292830322,37.2856232296221,38.2729536289223,39.2602840282224,
40.2476144275226,40.8407044966673),.UNSPECIFIED.);
#297=B_SPLINE_CURVE_WITH_KNOTS('',3,(#8392,#8393,#8394,#8395,#8396,#8397,
#8398,#8399,#8400,#8401),.UNSPECIFIED.,.F.,.F.,(4,1,1,1,1,1,1,4),(34.5575191894877,
34.9987850329832,35.9873519767085,36.9759189204337,37.964485864159,38.9530528078842,
39.9416197516095,40.8407044966673),.UNSPECIFIED.);
#298=B_SPLINE_CURVE_WITH_KNOTS('',3,(#8406,#8407,#8408,#8409,#8410,#8411,
#8412,#8413,#8414,#8415,#8416),.UNSPECIFIED.,.F.,.F.,(4,1,1,1,1,1,1,1,4),
(28.2743338823081,28.3996496359208,29.3869800352209,30.3743104345211,31.3616408338212,
32.3489712331214,33.3363016324215,34.3236320317217,34.5575191894877),
 .UNSPECIFIED.);
#299=B_SPLINE_CURVE_WITH_KNOTS('',3,(#8417,#8418,#8419,#8420,#8421,#8422,
#8423,#8424,#8425,#8426),.UNSPECIFIED.,.F.,.F.,(4,1,1,1,1,1,1,4),(28.2743338823081,
29.0673833706316,30.0559503143569,31.0445172580821,32.0330842018074,33.0216511455327,
34.0102180892579,34.5575191894877),.UNSPECIFIED.);
#300=B_SPLINE_CURVE_WITH_KNOTS('',3,(#8431,#8432,#8433,#8434,#8435,#8436,
#8437,#8438,#8439,#8440),.UNSPECIFIED.,.F.,.F.,(4,1,1,1,1,1,1,4),(21.9911485751285,
22.4756672401199,23.46299763942,24.4503280387202,25.4376584380203,26.4249888373205,
27.4123192366206,28.2743338823081),.UNSPECIFIED.);
#301=B_SPLINE_CURVE_WITH_KNOTS('',3,(#8441,#8442,#8443,#8444,#8445,#8446,
#8447,#8448,#8449,#8450,#8451),.UNSPECIFIED.,.F.,.F.,(4,1,1,1,1,1,1,1,4),
(21.9911485751285,22.1474147645547,23.13598170828,24.1245486520053,25.1131155957305,
26.1016825394558,27.0902494831811,28.0788164269063,28.2743338823081),
 .UNSPECIFIED.);
#302=B_SPLINE_CURVE_WITH_KNOTS('',3,(#8456,#8457,#8458,#8459,#8460,#8461,
#8462,#8463,#8464,#8465),.UNSPECIFIED.,.F.,.F.,(4,1,1,1,1,1,1,4),(15.7079632679489,
16.551684844319,17.5390152436191,18.5263456429193,19.5136760422194,20.5010064415196,
21.4883368408197,21.9911485751285),.UNSPECIFIED.);
#303=B_SPLINE_CURVE_WITH_KNOTS('',3,(#8466,#8467,#8468,#8469,#8470,#8471,
#8472,#8473,#8474,#8475),.UNSPECIFIED.,.F.,.F.,(4,1,1,1,1,1,1,4),(15.7079632679489,
16.2160131022032,17.2045800459284,18.1931469896537,19.181713933379,20.1702808771042,
21.1588478208295,21.9911485751285),.UNSPECIFIED.);
#304=B_SPLINE_CURVE_WITH_KNOTS('',3,(#8478,#8479,#8480,#8481,#8482,#8483,
#8484,#8485,#8486,#8487,#8488,#8489,#8490,#8491,#8492,#8493,#8494,#8495,
#8496,#8497,#8498,#8499,#8500,#8501,#8502,#8503,#8504,#8505,#8506,#8507,
#8508,#8509,#8510,#8511,#8512,#8513,#8514,#8515,#8516,#8517,#8518,#8519,
#8520,#8521,#8522,#8523,#8524,#8525,#8526,#8527,#8528,#8529,#8530,#8531,
#8532,#8533,#8534,#8535,#8536,#8537,#8538,#8539,#8540,#8541,#8542,#8543,
#8544,#8545,#8546,#8547,#8548,#8549,#8550,#8551,#8552,#8553,#8554,#8555,
#8556,#8557,#8558,#8559,#8560,#8561,#8562,#8563,#8564,#8565,#8566,#8567,
#8568,#8569,#8570,#8571,#8572,#8573,#8574,#8575,#8576,#8577,#8578,#8579,
#8580,#8581,#8582,#8583,#8584,#8585,#8586,#8587,#8588,#8589,#8590,#8591,
#8592,#8593,#8594,#8595,#8596,#8597,#8598,#8599,#8600,#8601,#8602,#8603,
#8604,#8605,#8606,#8607,#8608,#8609,#8610,#8611,#8612,#8613,#8614,#8615,
#8616,#8617,#8618,#8619,#8620,#8621,#8622,#8623,#8624,#8625,#8626,#8627,
#8628,#8629,#8630,#8631,#8632,#8633,#8634,#8635,#8636,#8637,#8638,#8639,
#8640,#8641,#8642,#8643,#8644,#8645,#8646,#8647,#8648,#8649,#8650,#8651,
#8652,#8653,#8654,#8655,#8656,#8657,#8658,#8659,#8660,#8661,#8662,#8663,
#8664,#8665,#8666,#8667,#8668,#8669,#8670,#8671,#8672,#8673,#8674,#8675,
#8676,#8677,#8678,#8679,#8680,#8681,#8682,#8683,#8684,#8685,#8686,#8687,
#8688,#8689,#8690,#8691,#8692,#8693,#8694),.UNSPECIFIED.,.F.,.F.,(4,3,3,
3,3,3,3,3,3,3,3,3,3,3,3,3,3,3,3,3,3,3,3,3,3,3,3,3,3,3,3,3,3,3,3,3,3,3,3,
3,3,3,3,3,3,3,3,3,3,3,3,3,3,3,3,3,3,3,3,3,3,3,3,3,3,3,3,3,3,3,3,3,4),(-1.51155304937228,
-1.48679174718013,-1.46137597198077,-1.44942691521821,-1.44205848651244,
-1.43724119559823,-1.41130764113729,-1.38514768961224,-1.36936593028954,
-1.36512230166791,-1.33867581137855,-1.31235917608035,-1.29127511993008,
-1.28073309185494,-1.2739086628828,-1.27019106377981,-1.24488979836553,
-1.21884130205047,-1.19384888620637,-1.18291470427457,-1.17641188206357,
-1.17130697868968,-1.14451640582175,-1.11742561305122,-1.09279470361283,
-1.08177565945417,-1.07670730294613,-1.07245364414871,-1.0452101587782,
-1.01890197529764,-0.992076665792053,-0.977095538498891,-0.971310437727824,
-0.944262984582137,-0.91671696123902,-0.889051349044572,-0.8786107219546,
-0.873404326505122,-0.869185758667877,-0.841205731090746,-0.813331817877821,
-0.785648584359967,-0.771436006282574,-0.765308450445371,-0.757965350842113,
-0.731019445974318,-0.703340715547858,-0.676331238706378,-0.668063308133434,
-0.663247880961674,-0.658967945513649,-0.630690110839631,-0.602089962339152,
-0.573383696958367,-0.562618847440572,-0.556352694911719,-0.55203012393032,
-0.523164492059728,-0.494713544949419,-0.487264900816012,-0.45884309987075,
-0.449622389577847,-0.445165938771905,-0.416742684601646,-0.387755299334011,
-0.358563756837841,-0.34211828207705,-0.337697582134308,-0.308241853281341,
-0.278784672736061,-0.25000255453776,-0.226999958751515,-0.219677966288006),
 .UNSPECIFIED.);
#305=B_SPLINE_CURVE_WITH_KNOTS('',3,(#8696,#8697,#8698,#8699,#8700,#8701,
#8702,#8703,#8704,#8705,#8706,#8707,#8708,#8709,#8710,#8711,#8712,#8713,
#8714,#8715,#8716,#8717,#8718,#8719,#8720,#8721,#8722,#8723,#8724,#8725,
#8726,#8727,#8728,#8729,#8730,#8731,#8732,#8733,#8734,#8735,#8736,#8737,
#8738,#8739,#8740,#8741,#8742,#8743,#8744,#8745,#8746,#8747,#8748,#8749,
#8750,#8751,#8752,#8753,#8754,#8755,#8756),.UNSPECIFIED.,.F.,.F.,(4,3,3,
3,3,3,3,3,3,3,3,3,3,3,3,3,3,3,3,3,4),(-0.410648750432938,-0.381294613665594,
-0.352267124576947,-0.328792823836752,-0.311187098281605,-0.306018425011984,
-0.301691296836585,-0.274143229574461,-0.258369921616165,-0.230117472373342,
-0.201352788326674,-0.195525900786732,-0.16833922287309,-0.141249160586392,
-0.114615533759621,-0.100282139063474,-0.0960342097686789,-0.0702554174629941,
-0.0448546715641945,-0.0201984500449382,0.),.UNSPECIFIED.);
#306=B_SPLINE_CURVE_WITH_KNOTS('',3,(#8759,#8760,#8761,#8762,#8763,#8764,
#8765,#8766,#8767,#8768,#8769,#8770,#8771,#8772,#8773,#8774,#8775,#8776,
#8777,#8778,#8779,#8780,#8781,#8782,#8783,#8784,#8785,#8786,#8787,#8788,
#8789),.UNSPECIFIED.,.F.,.F.,(4,3,3,3,3,3,3,3,3,3,4),(-0.219677966288006,
-0.206985183547511,-0.178213580556878,-0.148819200354015,-0.130216800309763,
-0.118450459252591,-0.113866160083042,-0.0841488051349767,-0.0540951018364117,
-0.0242019686830237,0.),.UNSPECIFIED.);
#307=B_SPLINE_CURVE_WITH_KNOTS('',3,(#9102,#9103,#9104,#9105,#9106,#9107,
#9108,#9109),.UNSPECIFIED.,.F.,.F.,(4,1,1,1,1,4),(11.6150328478182,12.6023632471184,
13.5896936464185,14.5770240457187,15.5643544450188,15.7079632679489),
 .UNSPECIFIED.);
#308=B_SPLINE_CURVE_WITH_KNOTS('',3,(#9110,#9111,#9112,#9113,#9114,#9115,
#9116,#9117,#9118,#9119,#9120,#9121,#9122,#9123,#9124,#9125,#9126,#9127,
#9128,#9129,#9130,#9131,#9132,#9133,#9134,#9135,#9136,#9137,#9138,#9139,
#9140,#9141,#9142,#9143,#9144,#9145,#9146,#9147,#9148,#9149,#9150,#9151,
#9152,#9153,#9154,#9155,#9156,#9157,#9158,#9159,#9160,#9161,#9162,#9163,
#9164,#9165,#9166,#9167,#9168,#9169,#9170,#9171,#9172,#9173,#9174,#9175,
#9176,#9177,#9178,#9179,#9180,#9181,#9182,#9183,#9184,#9185,#9186,#9187,
#9188,#9189,#9190,#9191,#9192,#9193,#9194,#9195,#9196,#9197),
 .UNSPECIFIED.,.F.,.F.,(4,3,3,3,3,3,3,3,3,3,3,3,3,3,3,3,3,3,3,3,3,3,3,3,
3,3,3,3,3,4),(-0.55274537837504,-0.525174630400016,-0.495740003900857,-0.479498227927527,
-0.472105972866577,-0.443064611280178,-0.418881458903182,-0.408301329738247,
-0.401969450637142,-0.397429868442983,-0.369124488132221,-0.341064938672273,
-0.313899750226951,-0.29772704364586,-0.291366968188088,-0.264559598151202,
-0.249599392264211,-0.222215347947115,-0.194438429453726,-0.189292991414398,
-0.162670593649827,-0.136062352557756,-0.109859916217256,-0.101879142728474,
-0.0950850259724172,-0.09115324392662,-0.0655931049079899,-0.0404250325776628,
-0.0160423336449029,0.),.UNSPECIFIED.);
#309=B_SPLINE_CURVE_WITH_KNOTS('',3,(#9198,#9199,#9200,#9201,#9202,#9203,
#9204,#9205,#9206,#9207,#9208,#9209,#9210,#9211,#9212,#9213,#9214,#9215,
#9216),.UNSPECIFIED.,.F.,.F.,(4,3,3,3,3,3,4),(-71.548101301701,-71.0877887496107,
-70.1004583503106,-69.1131279510104,-68.1257975517103,-67.1384671524101,
-66.9247834919266),.UNSPECIFIED.);
#310=B_SPLINE_CURVE_WITH_KNOTS('',3,(#9219,#9220,#9221,#9222,#9223,#9224,
#9225,#9226,#9227),.UNSPECIFIED.,.F.,.F.,(4,1,1,1,1,1,4),(10.3761157273102,
11.2731783835768,12.2617453273021,13.2503122710274,14.2388792147526,15.2274461584779,
15.7079632679489),.UNSPECIFIED.);
#311=B_SPLINE_CURVE_WITH_KNOTS('',3,(#9545,#9546,#9547,#9548,#9549,#9550,
#9551,#9552,#9553,#9554,#9555,#9556,#9557,#9558,#9559,#9560,#9561,#9562,
#9563,#9564,#9565,#9566),.UNSPECIFIED.,.F.,.F.,(4,3,3,3,3,3,3,4),(63.9491534801641,
64.2568513421422,65.2454182858675,66.2339852295928,67.222552173318,68.2111191170433,
69.1996860607685,69.4794631267919),.UNSPECIFIED.);
#312=B_SPLINE_CURVE_WITH_KNOTS('',3,(#9567,#9568,#9569,#9570,#9571,#9572,
#9573,#9574,#9575,#9576,#9577,#9578,#9579,#9580,#9581,#9582,#9583,#9584,
#9585,#9586,#9587,#9588,#9589,#9590,#9591,#9592,#9593,#9594,#9595,#9596,
#9597,#9598,#9599,#9600,#9601,#9602,#9603,#9604,#9605,#9606,#9607,#9608,
#9609,#9610,#9611,#9612,#9613,#9614,#9615,#9616,#9617,#9618,#9619,#9620,
#9621,#9622,#9623,#9624,#9625,#9626,#9627,#9628,#9629,#9630,#9631,#9632,
#9633,#9634,#9635,#9636,#9637,#9638,#9639,#9640,#9641,#9642,#9643,#9644,
#9645,#9646,#9647,#9648,#9649,#9650,#9651,#9652,#9653,#9654),
 .UNSPECIFIED.,.F.,.F.,(4,3,3,3,3,3,3,3,3,3,3,3,3,3,3,3,3,3,3,3,3,3,3,3,
3,3,3,3,3,4),(-0.555272788399385,-0.533197712400843,-0.50841200558917,-0.492097097422296,
-0.487698425831477,-0.461722637175749,-0.438993822101987,-0.427671428401512,
-0.42202191869945,-0.395458071621424,-0.368431943977533,-0.346296987129563,
-0.329695769493585,-0.32517826205158,-0.321068892319616,-0.293156561268766,
-0.279892116585652,-0.25291117159626,-0.225403496298925,-0.221057334466692,
-0.216708298034074,-0.188764735094145,-0.160284152968102,-0.131561788206246,
-0.114355289595352,-0.109564750157472,-0.0800994390258527,-0.050557237845911,
-0.0215776241374192,0.),.UNSPECIFIED.);
#313=SHAPE_REPRESENTATION_RELATIONSHIP('SRR','None',#9857,#324);
#314=SHAPE_REPRESENTATION_RELATIONSHIP('SRR','None',#9858,#325);
#315=SHAPE_REPRESENTATION_RELATIONSHIP('SRR','None',#9859,#326);
#316=SHAPE_REPRESENTATION_RELATIONSHIP('SRR','None',#9860,#327);
#317=SHAPE_REPRESENTATION_RELATIONSHIP('SRR','None',#9861,#328);
#318=SHAPE_REPRESENTATION_RELATIONSHIP('SRR','None',#9862,#329);
#319=SHAPE_REPRESENTATION_RELATIONSHIP('SRR','None',#9863,#330);
#320=SHAPE_REPRESENTATION_RELATIONSHIP('SRR','None',#9864,#331);
#321=SHAPE_REPRESENTATION_RELATIONSHIP('SRR','None',#9865,#332);
#322=SHAPE_REPRESENTATION_RELATIONSHIP('SRR','None',#9866,#333);
#323=SHAPE_REPRESENTATION_RELATIONSHIP('SRR','None',#9867,#334);
#324=ADVANCED_BREP_SHAPE_REPRESENTATION('',(#346),#9766);
#325=ADVANCED_BREP_SHAPE_REPRESENTATION('',(#347),#9767);
#326=ADVANCED_BREP_SHAPE_REPRESENTATION('',(#348),#9768);
#327=ADVANCED_BREP_SHAPE_REPRESENTATION('',(#349),#9769);
#328=ADVANCED_BREP_SHAPE_REPRESENTATION('',(#350),#9770);
#329=ADVANCED_BREP_SHAPE_REPRESENTATION('',(#351),#9771);
#330=ADVANCED_BREP_SHAPE_REPRESENTATION('',(#352),#9772);
#331=ADVANCED_BREP_SHAPE_REPRESENTATION('',(#353),#9773);
#332=ADVANCED_BREP_SHAPE_REPRESENTATION('',(#354),#9774);
#333=ADVANCED_BREP_SHAPE_REPRESENTATION('',(#355),#9775);
#334=ADVANCED_BREP_SHAPE_REPRESENTATION('',(#356),#9776);
#335=STYLED_ITEM('',(#9921),#346);
#336=STYLED_ITEM('',(#9922),#347);
#337=STYLED_ITEM('',(#9922),#348);
#338=STYLED_ITEM('',(#9923),#349);
#339=STYLED_ITEM('',(#9924),#350);
#340=STYLED_ITEM('',(#9925),#351);
#341=STYLED_ITEM('',(#9926),#352);
#342=STYLED_ITEM('',(#9927),#353);
#343=STYLED_ITEM('',(#9928),#354);
#344=STYLED_ITEM('',(#9929),#355);
#345=STYLED_ITEM('',(#9930),#356);
#346=MANIFOLD_SOLID_BREP('Aluminum square hollow profile',#3840);
#347=MANIFOLD_SOLID_BREP('Aluminum square hollow profile',#3841);
#348=MANIFOLD_SOLID_BREP('Aluminum square hollow profile',#3842);
#349=MANIFOLD_SOLID_BREP('Aluminum channel profile',#3843);
#350=MANIFOLD_SOLID_BREP('Body1',#3844);
#351=MANIFOLD_SOLID_BREP('Body1',#3845);
#352=MANIFOLD_SOLID_BREP('Body1',#3846);
#353=MANIFOLD_SOLID_BREP('Body1',#3847);
#354=MANIFOLD_SOLID_BREP('Body1',#3848);
#355=MANIFOLD_SOLID_BREP('Body1',#3849);
#356=MANIFOLD_SOLID_BREP('Body1',#3850);
#357=FACE_BOUND('',#703,.T.);
#358=FACE_BOUND('',#719,.T.);
#359=FACE_BOUND('',#725,.T.);
#360=FACE_BOUND('',#732,.T.);
#361=FACE_BOUND('',#733,.T.);
#362=FACE_BOUND('',#741,.T.);
#363=FACE_BOUND('',#742,.T.);
#364=FACE_BOUND('',#745,.T.);
#365=FACE_BOUND('',#749,.T.);
#366=FACE_BOUND('',#765,.T.);
#367=FACE_BOUND('',#771,.T.);
#368=FACE_BOUND('',#772,.T.);
#369=FACE_BOUND('',#779,.T.);
#370=FACE_BOUND('',#780,.T.);
#371=FACE_BOUND('',#809,.T.);
#372=FACE_BOUND('',#810,.T.);
#373=FACE_BOUND('',#811,.T.);
#374=FACE_BOUND('',#812,.T.);
#375=FACE_BOUND('',#813,.T.);
#376=FACE_BOUND('',#814,.T.);
#377=FACE_BOUND('',#815,.T.);
#378=FACE_BOUND('',#816,.T.);
#379=FACE_BOUND('',#818,.T.);
#380=FACE_BOUND('',#819,.T.);
#381=FACE_BOUND('',#820,.T.);
#382=FACE_BOUND('',#821,.T.);
#383=FACE_BOUND('',#822,.T.);
#384=FACE_BOUND('',#823,.T.);
#385=FACE_BOUND('',#824,.T.);
#386=FACE_BOUND('',#825,.T.);
#387=FACE_BOUND('',#837,.T.);
#388=FACE_BOUND('',#838,.T.);
#389=FACE_BOUND('',#839,.T.);
#390=FACE_BOUND('',#840,.T.);
#391=FACE_BOUND('',#842,.T.);
#392=FACE_BOUND('',#843,.T.);
#393=FACE_BOUND('',#844,.T.);
#394=FACE_BOUND('',#845,.T.);
#395=FACE_BOUND('',#855,.T.);
#396=FACE_BOUND('',#856,.T.);
#397=FACE_BOUND('',#857,.T.);
#398=FACE_BOUND('',#858,.T.);
#399=FACE_BOUND('',#860,.T.);
#400=FACE_BOUND('',#861,.T.);
#401=FACE_BOUND('',#862,.T.);
#402=FACE_BOUND('',#863,.T.);
#403=FACE_BOUND('',#897,.T.);
#404=FACE_BOUND('',#899,.T.);
#405=FACE_BOUND('',#901,.T.);
#406=FACE_BOUND('',#905,.T.);
#407=FACE_BOUND('',#910,.T.);
#408=FACE_BOUND('',#946,.T.);
#409=FACE_BOUND('',#949,.T.);
#410=PLANE('',#3978);
#411=PLANE('',#3979);
#412=PLANE('',#3989);
#413=PLANE('',#3996);
#414=PLANE('',#3999);
#415=PLANE('',#4002);
#416=PLANE('',#4005);
#417=PLANE('',#4006);
#418=PLANE('',#4007);
#419=PLANE('',#4008);
#420=PLANE('',#4019);
#421=PLANE('',#4020);
#422=PLANE('',#4030);
#423=PLANE('',#4037);
#424=PLANE('',#4040);
#425=PLANE('',#4043);
#426=PLANE('',#4046);
#427=PLANE('',#4047);
#428=PLANE('',#4048);
#429=PLANE('',#4049);
#430=PLANE('',#4054);
#431=PLANE('',#4055);
#432=PLANE('',#4065);
#433=PLANE('',#4072);
#434=PLANE('',#4075);
#435=PLANE('',#4078);
#436=PLANE('',#4081);
#437=PLANE('',#4082);
#438=PLANE('',#4083);
#439=PLANE('',#4084);
#440=PLANE('',#4095);
#441=PLANE('',#4103);
#442=PLANE('',#4108);
#443=PLANE('',#4113);
#444=PLANE('',#4116);
#445=PLANE('',#4121);
#446=PLANE('',#4122);
#447=PLANE('',#4123);
#448=PLANE('',#4124);
#449=PLANE('',#4125);
#450=PLANE('',#4151);
#451=PLANE('',#4152);
#452=PLANE('',#4153);
#453=PLANE('',#4154);
#454=PLANE('',#4155);
#455=PLANE('',#4156);
#456=PLANE('',#4157);
#457=PLANE('',#4158);
#458=PLANE('',#4159);
#459=PLANE('',#4160);
#460=PLANE('',#4161);
#461=PLANE('',#4162);
#462=PLANE('',#4163);
#463=PLANE('',#4164);
#464=PLANE('',#4178);
#465=PLANE('',#4179);
#466=PLANE('',#4180);
#467=PLANE('',#4181);
#468=PLANE('',#4182);
#469=PLANE('',#4183);
#470=PLANE('',#4197);
#471=PLANE('',#4198);
#472=PLANE('',#4199);
#473=PLANE('',#4200);
#474=PLANE('',#4201);
#475=PLANE('',#4202);
#476=PLANE('',#4204);
#477=PLANE('',#4205);
#478=PLANE('',#4206);
#479=PLANE('',#4207);
#480=PLANE('',#4208);
#481=PLANE('',#4209);
#482=PLANE('',#4211);
#483=PLANE('',#4212);
#484=PLANE('',#4213);
#485=PLANE('',#4214);
#486=PLANE('',#4215);
#487=PLANE('',#4240);
#488=PLANE('',#4242);
#489=PLANE('',#4245);
#490=PLANE('',#4251);
#491=PLANE('',#4257);
#492=PLANE('',#4289);
#493=PLANE('',#4290);
#494=PLANE('',#4291);
#495=PLANE('',#4292);
#496=PLANE('',#4293);
#497=PLANE('',#4294);
#498=PLANE('',#4295);
#499=PLANE('',#4296);
#500=PLANE('',#4300);
#501=PLANE('',#4301);
#502=FACE_OUTER_BOUND('',#700,.T.);
#503=FACE_OUTER_BOUND('',#701,.T.);
#504=FACE_OUTER_BOUND('',#702,.T.);
#505=FACE_OUTER_BOUND('',#704,.T.);
#506=FACE_OUTER_BOUND('',#705,.T.);
#507=FACE_OUTER_BOUND('',#706,.T.);
#508=FACE_OUTER_BOUND('',#707,.T.);
#509=FACE_OUTER_BOUND('',#708,.T.);
#510=FACE_OUTER_BOUND('',#709,.T.);
#511=FACE_OUTER_BOUND('',#710,.T.);
#512=FACE_OUTER_BOUND('',#711,.T.);
#513=FACE_OUTER_BOUND('',#712,.T.);
#514=FACE_OUTER_BOUND('',#713,.T.);
#515=FACE_OUTER_BOUND('',#714,.T.);
#516=FACE_OUTER_BOUND('',#715,.T.);
#517=FACE_OUTER_BOUND('',#716,.T.);
#518=FACE_OUTER_BOUND('',#717,.T.);
#519=FACE_OUTER_BOUND('',#718,.T.);
#520=FACE_OUTER_BOUND('',#720,.T.);
#521=FACE_OUTER_BOUND('',#721,.T.);
#522=FACE_OUTER_BOUND('',#722,.T.);
#523=FACE_OUTER_BOUND('',#723,.T.);
#524=FACE_OUTER_BOUND('',#724,.T.);
#525=FACE_OUTER_BOUND('',#726,.T.);
#526=FACE_OUTER_BOUND('',#727,.T.);
#527=FACE_OUTER_BOUND('',#728,.T.);
#528=FACE_OUTER_BOUND('',#729,.T.);
#529=FACE_OUTER_BOUND('',#730,.T.);
#530=FACE_OUTER_BOUND('',#731,.T.);
#531=FACE_OUTER_BOUND('',#734,.T.);
#532=FACE_OUTER_BOUND('',#735,.T.);
#533=FACE_OUTER_BOUND('',#736,.T.);
#534=FACE_OUTER_BOUND('',#737,.T.);
#535=FACE_OUTER_BOUND('',#738,.T.);
#536=FACE_OUTER_BOUND('',#739,.T.);
#537=FACE_OUTER_BOUND('',#740,.T.);
#538=FACE_OUTER_BOUND('',#743,.T.);
#539=FACE_OUTER_BOUND('',#744,.T.);
#540=FACE_OUTER_BOUND('',#746,.T.);
#541=FACE_OUTER_BOUND('',#747,.T.);
#542=FACE_OUTER_BOUND('',#748,.T.);
#543=FACE_OUTER_BOUND('',#750,.T.);
#544=FACE_OUTER_BOUND('',#751,.T.);
#545=FACE_OUTER_BOUND('',#752,.T.);
#546=FACE_OUTER_BOUND('',#753,.T.);
#547=FACE_OUTER_BOUND('',#754,.T.);
#548=FACE_OUTER_BOUND('',#755,.T.);
#549=FACE_OUTER_BOUND('',#756,.T.);
#550=FACE_OUTER_BOUND('',#757,.T.);
#551=FACE_OUTER_BOUND('',#758,.T.);
#552=FACE_OUTER_BOUND('',#759,.T.);
#553=FACE_OUTER_BOUND('',#760,.T.);
#554=FACE_OUTER_BOUND('',#761,.T.);
#555=FACE_OUTER_BOUND('',#762,.T.);
#556=FACE_OUTER_BOUND('',#763,.T.);
#557=FACE_OUTER_BOUND('',#764,.T.);
#558=FACE_OUTER_BOUND('',#766,.T.);
#559=FACE_OUTER_BOUND('',#767,.T.);
#560=FACE_OUTER_BOUND('',#768,.T.);
#561=FACE_OUTER_BOUND('',#769,.T.);
#562=FACE_OUTER_BOUND('',#770,.T.);
#563=FACE_OUTER_BOUND('',#773,.T.);
#564=FACE_OUTER_BOUND('',#774,.T.);
#565=FACE_OUTER_BOUND('',#775,.T.);
#566=FACE_OUTER_BOUND('',#776,.T.);
#567=FACE_OUTER_BOUND('',#777,.T.);
#568=FACE_OUTER_BOUND('',#778,.T.);
#569=FACE_OUTER_BOUND('',#781,.T.);
#570=FACE_OUTER_BOUND('',#782,.T.);
#571=FACE_OUTER_BOUND('',#783,.T.);
#572=FACE_OUTER_BOUND('',#784,.T.);
#573=FACE_OUTER_BOUND('',#785,.T.);
#574=FACE_OUTER_BOUND('',#786,.T.);
#575=FACE_OUTER_BOUND('',#787,.T.);
#576=FACE_OUTER_BOUND('',#788,.T.);
#577=FACE_OUTER_BOUND('',#789,.T.);
#578=FACE_OUTER_BOUND('',#790,.T.);
#579=FACE_OUTER_BOUND('',#791,.T.);
#580=FACE_OUTER_BOUND('',#792,.T.);
#581=FACE_OUTER_BOUND('',#793,.T.);
#582=FACE_OUTER_BOUND('',#794,.T.);
#583=FACE_OUTER_BOUND('',#795,.T.);
#584=FACE_OUTER_BOUND('',#796,.T.);
#585=FACE_OUTER_BOUND('',#797,.T.);
#586=FACE_OUTER_BOUND('',#798,.T.);
#587=FACE_OUTER_BOUND('',#799,.T.);
#588=FACE_OUTER_BOUND('',#800,.T.);
#589=FACE_OUTER_BOUND('',#801,.T.);
#590=FACE_OUTER_BOUND('',#802,.T.);
#591=FACE_OUTER_BOUND('',#803,.T.);
#592=FACE_OUTER_BOUND('',#804,.T.);
#593=FACE_OUTER_BOUND('',#805,.T.);
#594=FACE_OUTER_BOUND('',#806,.T.);
#595=FACE_OUTER_BOUND('',#807,.T.);
#596=FACE_OUTER_BOUND('',#808,.T.);
#597=FACE_OUTER_BOUND('',#817,.T.);
#598=FACE_OUTER_BOUND('',#826,.T.);
#599=FACE_OUTER_BOUND('',#827,.T.);
#600=FACE_OUTER_BOUND('',#828,.T.);
#601=FACE_OUTER_BOUND('',#829,.T.);
#602=FACE_OUTER_BOUND('',#830,.T.);
#603=FACE_OUTER_BOUND('',#831,.T.);
#604=FACE_OUTER_BOUND('',#832,.T.);
#605=FACE_OUTER_BOUND('',#833,.T.);
#606=FACE_OUTER_BOUND('',#834,.T.);
#607=FACE_OUTER_BOUND('',#835,.T.);
#608=FACE_OUTER_BOUND('',#836,.T.);
#609=FACE_OUTER_BOUND('',#841,.T.);
#610=FACE_OUTER_BOUND('',#846,.T.);
#611=FACE_OUTER_BOUND('',#847,.T.);
#612=FACE_OUTER_BOUND('',#848,.T.);
#613=FACE_OUTER_BOUND('',#849,.T.);
#614=FACE_OUTER_BOUND('',#850,.T.);
#615=FACE_OUTER_BOUND('',#851,.T.);
#616=FACE_OUTER_BOUND('',#852,.T.);
#617=FACE_OUTER_BOUND('',#853,.T.);
#618=FACE_OUTER_BOUND('',#854,.T.);
#619=FACE_OUTER_BOUND('',#859,.T.);
#620=FACE_OUTER_BOUND('',#864,.T.);
#621=FACE_OUTER_BOUND('',#865,.T.);
#622=FACE_OUTER_BOUND('',#866,.T.);
#623=FACE_OUTER_BOUND('',#867,.T.);
#624=FACE_OUTER_BOUND('',#868,.T.);
#625=FACE_OUTER_BOUND('',#869,.T.);
#626=FACE_OUTER_BOUND('',#870,.T.);
#627=FACE_OUTER_BOUND('',#871,.T.);
#628=FACE_OUTER_BOUND('',#872,.T.);
#629=FACE_OUTER_BOUND('',#873,.T.);
#630=FACE_OUTER_BOUND('',#874,.T.);
#631=FACE_OUTER_BOUND('',#875,.T.);
#632=FACE_OUTER_BOUND('',#876,.T.);
#633=FACE_OUTER_BOUND('',#877,.T.);
#634=FACE_OUTER_BOUND('',#878,.T.);
#635=FACE_OUTER_BOUND('',#879,.T.);
#636=FACE_OUTER_BOUND('',#880,.T.);
#637=FACE_OUTER_BOUND('',#881,.T.);
#638=FACE_OUTER_BOUND('',#882,.T.);
#639=FACE_OUTER_BOUND('',#883,.T.);
#640=FACE_OUTER_BOUND('',#884,.T.);
#641=FACE_OUTER_BOUND('',#885,.T.);
#642=FACE_OUTER_BOUND('',#886,.T.);
#643=FACE_OUTER_BOUND('',#887,.T.);
#644=FACE_OUTER_BOUND('',#888,.T.);
#645=FACE_OUTER_BOUND('',#889,.T.);
#646=FACE_OUTER_BOUND('',#890,.T.);
#647=FACE_OUTER_BOUND('',#891,.T.);
#648=FACE_OUTER_BOUND('',#892,.T.);
#649=FACE_OUTER_BOUND('',#893,.T.);
#650=FACE_OUTER_BOUND('',#894,.T.);
#651=FACE_OUTER_BOUND('',#895,.T.);
#652=FACE_OUTER_BOUND('',#896,.T.);
#653=FACE_OUTER_BOUND('',#898,.T.);
#654=FACE_OUTER_BOUND('',#900,.T.);
#655=FACE_OUTER_BOUND('',#902,.T.);
#656=FACE_OUTER_BOUND('',#903,.T.);
#657=FACE_OUTER_BOUND('',#904,.T.);
#658=FACE_OUTER_BOUND('',#906,.T.);
#659=FACE_OUTER_BOUND('',#907,.T.);
#660=FACE_OUTER_BOUND('',#908,.T.);
#661=FACE_OUTER_BOUND('',#909,.T.);
#662=FACE_OUTER_BOUND('',#911,.T.);
#663=FACE_OUTER_BOUND('',#912,.T.);
#664=FACE_OUTER_BOUND('',#913,.T.);
#665=FACE_OUTER_BOUND('',#914,.T.);
#666=FACE_OUTER_BOUND('',#915,.T.);
#667=FACE_OUTER_BOUND('',#916,.T.);
#668=FACE_OUTER_BOUND('',#917,.T.);
#669=FACE_OUTER_BOUND('',#918,.T.);
#670=FACE_OUTER_BOUND('',#919,.T.);
#671=FACE_OUTER_BOUND('',#920,.T.);
#672=FACE_OUTER_BOUND('',#921,.T.);
#673=FACE_OUTER_BOUND('',#922,.T.);
#674=FACE_OUTER_BOUND('',#923,.T.);
#675=FACE_OUTER_BOUND('',#924,.T.);
#676=FACE_OUTER_BOUND('',#925,.T.);
#677=FACE_OUTER_BOUND('',#926,.T.);
#678=FACE_OUTER_BOUND('',#927,.T.);
#679=FACE_OUTER_BOUND('',#928,.T.);
#680=FACE_OUTER_BOUND('',#929,.T.);
#681=FACE_OUTER_BOUND('',#930,.T.);
#682=FACE_OUTER_BOUND('',#931,.T.);
#683=FACE_OUTER_BOUND('',#932,.T.);
#684=FACE_OUTER_BOUND('',#933,.T.);
#685=FACE_OUTER_BOUND('',#934,.T.);
#686=FACE_OUTER_BOUND('',#935,.T.);
#687=FACE_OUTER_BOUND('',#936,.T.);
#688=FACE_OUTER_BOUND('',#937,.T.);
#689=FACE_OUTER_BOUND('',#938,.T.);
#690=FACE_OUTER_BOUND('',#939,.T.);
#691=FACE_OUTER_BOUND('',#940,.T.);
#692=FACE_OUTER_BOUND('',#941,.T.);
#693=FACE_OUTER_BOUND('',#942,.T.);
#694=FACE_OUTER_BOUND('',#943,.T.);
#695=FACE_OUTER_BOUND('',#944,.T.);
#696=FACE_OUTER_BOUND('',#945,.T.);
#697=FACE_OUTER_BOUND('',#947,.T.);
#698=FACE_OUTER_BOUND('',#948,.T.);
#699=FACE_OUTER_BOUND('',#950,.T.);
#700=EDGE_LOOP('',(#2515,#2516,#2517,#2518));
#701=EDGE_LOOP('',(#2519,#2520,#2521,#2522));
#702=EDGE_LOOP('',(#2523,#2524,#2525,#2526,#2527,#2528,#2529,#2530));
#703=EDGE_LOOP('',(#2531,#2532,#2533,#2534,#2535,#2536,#2537,#2538));
#704=EDGE_LOOP('',(#2539,#2540,#2541,#2542));
#705=EDGE_LOOP('',(#2543,#2544,#2545,#2546));
#706=EDGE_LOOP('',(#2547,#2548,#2549,#2550));
#707=EDGE_LOOP('',(#2551,#2552,#2553,#2554));
#708=EDGE_LOOP('',(#2555,#2556,#2557,#2558));
#709=EDGE_LOOP('',(#2559,#2560,#2561,#2562));
#710=EDGE_LOOP('',(#2563,#2564,#2565,#2566));
#711=EDGE_LOOP('',(#2567,#2568,#2569,#2570));
#712=EDGE_LOOP('',(#2571,#2572,#2573,#2574));
#713=EDGE_LOOP('',(#2575,#2576,#2577,#2578));
#714=EDGE_LOOP('',(#2579,#2580,#2581,#2582));
#715=EDGE_LOOP('',(#2583,#2584,#2585,#2586));
#716=EDGE_LOOP('',(#2587,#2588,#2589,#2590));
#717=EDGE_LOOP('',(#2591,#2592,#2593,#2594));
#718=EDGE_LOOP('',(#2595,#2596,#2597,#2598,#2599,#2600,#2601,#2602));
#719=EDGE_LOOP('',(#2603,#2604,#2605,#2606,#2607,#2608,#2609,#2610));
#720=EDGE_LOOP('',(#2611,#2612,#2613,#2614));
#721=EDGE_LOOP('',(#2615,#2616,#2617,#2618));
#722=EDGE_LOOP('',(#2619,#2620,#2621,#2622));
#723=EDGE_LOOP('',(#2623,#2624,#2625,#2626));
#724=EDGE_LOOP('',(#2627,#2628,#2629,#2630,#2631,#2632,#2633,#2634));
#725=EDGE_LOOP('',(#2635,#2636,#2637,#2638,#2639,#2640,#2641,#2642));
#726=EDGE_LOOP('',(#2643,#2644,#2645,#2646));
#727=EDGE_LOOP('',(#2647,#2648,#2649,#2650));
#728=EDGE_LOOP('',(#2651,#2652,#2653,#2654));
#729=EDGE_LOOP('',(#2655,#2656,#2657,#2658));
#730=EDGE_LOOP('',(#2659,#2660,#2661,#2662));
#731=EDGE_LOOP('',(#2663,#2664,#2665,#2666));
#732=EDGE_LOOP('',(#2667));
#733=EDGE_LOOP('',(#2668));
#734=EDGE_LOOP('',(#2669,#2670,#2671,#2672));
#735=EDGE_LOOP('',(#2673,#2674,#2675,#2676));
#736=EDGE_LOOP('',(#2677,#2678,#2679,#2680));
#737=EDGE_LOOP('',(#2681,#2682,#2683,#2684));
#738=EDGE_LOOP('',(#2685,#2686,#2687,#2688));
#739=EDGE_LOOP('',(#2689,#2690,#2691,#2692));
#740=EDGE_LOOP('',(#2693,#2694,#2695,#2696));
#741=EDGE_LOOP('',(#2697));
#742=EDGE_LOOP('',(#2698));
#743=EDGE_LOOP('',(#2699,#2700,#2701,#2702));
#744=EDGE_LOOP('',(#2703,#2704,#2705,#2706,#2707,#2708,#2709,#2710));
#745=EDGE_LOOP('',(#2711,#2712,#2713,#2714,#2715,#2716,#2717,#2718));
#746=EDGE_LOOP('',(#2719,#2720,#2721,#2722));
#747=EDGE_LOOP('',(#2723,#2724,#2725,#2726));
#748=EDGE_LOOP('',(#2727,#2728,#2729,#2730,#2731,#2732,#2733,#2734));
#749=EDGE_LOOP('',(#2735,#2736,#2737,#2738,#2739,#2740,#2741,#2742));
#750=EDGE_LOOP('',(#2743,#2744,#2745,#2746));
#751=EDGE_LOOP('',(#2747,#2748,#2749,#2750));
#752=EDGE_LOOP('',(#2751,#2752,#2753,#2754));
#753=EDGE_LOOP('',(#2755,#2756,#2757,#2758));
#754=EDGE_LOOP('',(#2759,#2760,#2761,#2762));
#755=EDGE_LOOP('',(#2763,#2764,#2765,#2766));
#756=EDGE_LOOP('',(#2767,#2768,#2769,#2770));
#757=EDGE_LOOP('',(#2771,#2772,#2773,#2774));
#758=EDGE_LOOP('',(#2775,#2776,#2777,#2778));
#759=EDGE_LOOP('',(#2779,#2780,#2781,#2782));
#760=EDGE_LOOP('',(#2783,#2784,#2785,#2786));
#761=EDGE_LOOP('',(#2787,#2788,#2789,#2790));
#762=EDGE_LOOP('',(#2791,#2792,#2793,#2794));
#763=EDGE_LOOP('',(#2795,#2796,#2797,#2798));
#764=EDGE_LOOP('',(#2799,#2800,#2801,#2802,#2803,#2804,#2805,#2806));
#765=EDGE_LOOP('',(#2807,#2808,#2809,#2810,#2811,#2812,#2813,#2814));
#766=EDGE_LOOP('',(#2815,#2816,#2817,#2818));
#767=EDGE_LOOP('',(#2819,#2820,#2821,#2822));
#768=EDGE_LOOP('',(#2823,#2824,#2825,#2826));
#769=EDGE_LOOP('',(#2827,#2828,#2829,#2830,#2831,#2832,#2833,#2834,#2835,
#2836,#2837,#2838,#2839,#2840,#2841,#2842));
#770=EDGE_LOOP('',(#2843,#2844,#2845,#2846));
#771=EDGE_LOOP('',(#2847));
#772=EDGE_LOOP('',(#2848));
#773=EDGE_LOOP('',(#2849,#2850,#2851,#2852));
#774=EDGE_LOOP('',(#2853,#2854,#2855,#2856));
#775=EDGE_LOOP('',(#2857,#2858,#2859,#2860));
#776=EDGE_LOOP('',(#2861,#2862,#2863,#2864));
#777=EDGE_LOOP('',(#2865,#2866,#2867,#2868));
#778=EDGE_LOOP('',(#2869,#2870,#2871,#2872));
#779=EDGE_LOOP('',(#2873));
#780=EDGE_LOOP('',(#2874));
#781=EDGE_LOOP('',(#2875,#2876,#2877,#2878));
#782=EDGE_LOOP('',(#2879,#2880,#2881,#2882));
#783=EDGE_LOOP('',(#2883,#2884,#2885,#2886));
#784=EDGE_LOOP('',(#2887,#2888,#2889,#2890));
#785=EDGE_LOOP('',(#2891,#2892,#2893,#2894));
#786=EDGE_LOOP('',(#2895,#2896,#2897,#2898));
#787=EDGE_LOOP('',(#2899,#2900,#2901,#2902));
#788=EDGE_LOOP('',(#2903,#2904,#2905,#2906));
#789=EDGE_LOOP('',(#2907,#2908,#2909,#2910,#2911,#2912,#2913,#2914,#2915,
#2916,#2917,#2918,#2919,#2920,#2921,#2922));
#790=EDGE_LOOP('',(#2923,#2924,#2925,#2926));
#791=EDGE_LOOP('',(#2927,#2928,#2929,#2930));
#792=EDGE_LOOP('',(#2931,#2932,#2933,#2934));
#793=EDGE_LOOP('',(#2935,#2936,#2937,#2938));
#794=EDGE_LOOP('',(#2939,#2940,#2941,#2942));
#795=EDGE_LOOP('',(#2943,#2944,#2945,#2946));
#796=EDGE_LOOP('',(#2947,#2948,#2949,#2950));
#797=EDGE_LOOP('',(#2951,#2952,#2953,#2954));
#798=EDGE_LOOP('',(#2955,#2956,#2957,#2958));
#799=EDGE_LOOP('',(#2959,#2960,#2961,#2962));
#800=EDGE_LOOP('',(#2963,#2964,#2965,#2966));
#801=EDGE_LOOP('',(#2967,#2968,#2969,#2970));
#802=EDGE_LOOP('',(#2971,#2972,#2973,#2974));
#803=EDGE_LOOP('',(#2975,#2976,#2977,#2978));
#804=EDGE_LOOP('',(#2979,#2980,#2981,#2982));
#805=EDGE_LOOP('',(#2983,#2984,#2985,#2986));
#806=EDGE_LOOP('',(#2987,#2988,#2989,#2990));
#807=EDGE_LOOP('',(#2991,#2992,#2993,#2994));
#808=EDGE_LOOP('',(#2995,#2996,#2997,#2998,#2999,#3000,#3001,#3002,#3003,
#3004,#3005,#3006));
#809=EDGE_LOOP('',(#3007));
#810=EDGE_LOOP('',(#3008));
#811=EDGE_LOOP('',(#3009));
#812=EDGE_LOOP('',(#3010));
#813=EDGE_LOOP('',(#3011));
#814=EDGE_LOOP('',(#3012));
#815=EDGE_LOOP('',(#3013));
#816=EDGE_LOOP('',(#3014));
#817=EDGE_LOOP('',(#3015,#3016,#3017,#3018,#3019,#3020,#3021,#3022,#3023,
#3024,#3025,#3026));
#818=EDGE_LOOP('',(#3027));
#819=EDGE_LOOP('',(#3028));
#820=EDGE_LOOP('',(#3029));
#821=EDGE_LOOP('',(#3030));
#822=EDGE_LOOP('',(#3031));
#823=EDGE_LOOP('',(#3032));
#824=EDGE_LOOP('',(#3033));
#825=EDGE_LOOP('',(#3034));
#826=EDGE_LOOP('',(#3035,#3036,#3037,#3038));
#827=EDGE_LOOP('',(#3039,#3040,#3041,#3042));
#828=EDGE_LOOP('',(#3043,#3044,#3045,#3046));
#829=EDGE_LOOP('',(#3047,#3048,#3049,#3050));
#830=EDGE_LOOP('',(#3051,#3052,#3053,#3054));
#831=EDGE_LOOP('',(#3055,#3056,#3057,#3058));
#832=EDGE_LOOP('',(#3059,#3060,#3061,#3062));
#833=EDGE_LOOP('',(#3063,#3064,#3065,#3066));
#834=EDGE_LOOP('',(#3067,#3068,#3069,#3070));
#835=EDGE_LOOP('',(#3071,#3072,#3073,#3074));
#836=EDGE_LOOP('',(#3075,#3076,#3077,#3078));
#837=EDGE_LOOP('',(#3079));
#838=EDGE_LOOP('',(#3080));
#839=EDGE_LOOP('',(#3081));
#840=EDGE_LOOP('',(#3082));
#841=EDGE_LOOP('',(#3083,#3084,#3085,#3086));
#842=EDGE_LOOP('',(#3087));
#843=EDGE_LOOP('',(#3088));
#844=EDGE_LOOP('',(#3089));
#845=EDGE_LOOP('',(#3090));
#846=EDGE_LOOP('',(#3091,#3092,#3093,#3094));
#847=EDGE_LOOP('',(#3095,#3096,#3097,#3098));
#848=EDGE_LOOP('',(#3099,#3100,#3101,#3102));
#849=EDGE_LOOP('',(#3103,#3104,#3105,#3106));
#850=EDGE_LOOP('',(#3107,#3108,#3109,#3110));
#851=EDGE_LOOP('',(#3111,#3112,#3113,#3114));
#852=EDGE_LOOP('',(#3115,#3116,#3117,#3118));
#853=EDGE_LOOP('',(#3119,#3120,#3121,#3122));
#854=EDGE_LOOP('',(#3123,#3124,#3125,#3126));
#855=EDGE_LOOP('',(#3127));
#856=EDGE_LOOP('',(#3128));
#857=EDGE_LOOP('',(#3129));
#858=EDGE_LOOP('',(#3130));
#859=EDGE_LOOP('',(#3131,#3132,#3133,#3134));
#860=EDGE_LOOP('',(#3135));
#861=EDGE_LOOP('',(#3136));
#862=EDGE_LOOP('',(#3137));
#863=EDGE_LOOP('',(#3138));
#864=EDGE_LOOP('',(#3139,#3140,#3141,#3142));
#865=EDGE_LOOP('',(#3143,#3144,#3145,#3146));
#866=EDGE_LOOP('',(#3147,#3148,#3149,#3150));
#867=EDGE_LOOP('',(#3151,#3152,#3153,#3154));
#868=EDGE_LOOP('',(#3155,#3156,#3157,#3158));
#869=EDGE_LOOP('',(#3159,#3160,#3161,#3162));
#870=EDGE_LOOP('',(#3163,#3164,#3165,#3166));
#871=EDGE_LOOP('',(#3167,#3168,#3169,#3170));
#872=EDGE_LOOP('',(#3171,#3172,#3173,#3174));
#873=EDGE_LOOP('',(#3175,#3176,#3177));
#874=EDGE_LOOP('',(#3178,#3179,#3180));
#875=EDGE_LOOP('',(#3181,#3182,#3183,#3184));
#876=EDGE_LOOP('',(#3185,#3186,#3187,#3188));
#877=EDGE_LOOP('',(#3189,#3190,#3191,#3192));
#878=EDGE_LOOP('',(#3193,#3194,#3195,#3196));
#879=EDGE_LOOP('',(#3197,#3198,#3199,#3200));
#880=EDGE_LOOP('',(#3201,#3202,#3203,#3204));
#881=EDGE_LOOP('',(#3205,#3206,#3207,#3208));
#882=EDGE_LOOP('',(#3209,#3210,#3211,#3212));
#883=EDGE_LOOP('',(#3213,#3214,#3215,#3216));
#884=EDGE_LOOP('',(#3217,#3218,#3219,#3220));
#885=EDGE_LOOP('',(#3221,#3222,#3223,#3224));
#886=EDGE_LOOP('',(#3225,#3226,#3227,#3228));
#887=EDGE_LOOP('',(#3229,#3230,#3231,#3232));
#888=EDGE_LOOP('',(#3233,#3234,#3235,#3236));
#889=EDGE_LOOP('',(#3237,#3238,#3239,#3240));
#890=EDGE_LOOP('',(#3241,#3242,#3243,#3244));
#891=EDGE_LOOP('',(#3245,#3246,#3247,#3248));
#892=EDGE_LOOP('',(#3249,#3250,#3251,#3252));
#893=EDGE_LOOP('',(#3253,#3254,#3255,#3256));
#894=EDGE_LOOP('',(#3257,#3258,#3259,#3260,#3261,#3262,#3263,#3264,#3265,
#3266,#3267,#3268,#3269,#3270,#3271,#3272,#3273,#3274,#3275,#3276,#3277,
#3278));
#895=EDGE_LOOP('',(#3279,#3280,#3281,#3282,#3283,#3284,#3285,#3286,#3287,
#3288,#3289,#3290,#3291,#3292,#3293,#3294,#3295,#3296,#3297,#3298,#3299,
#3300));
#896=EDGE_LOOP('',(#3301));
#897=EDGE_LOOP('',(#3302,#3303,#3304,#3305));
#898=EDGE_LOOP('',(#3306));
#899=EDGE_LOOP('',(#3307));
#900=EDGE_LOOP('',(#3308));
#901=EDGE_LOOP('',(#3309));
#902=EDGE_LOOP('',(#3310,#3311,#3312,#3313));
#903=EDGE_LOOP('',(#3314,#3315,#3316,#3317));
#904=EDGE_LOOP('',(#3318));
#905=EDGE_LOOP('',(#3319));
#906=EDGE_LOOP('',(#3320,#3321,#3322,#3323));
#907=EDGE_LOOP('',(#3324,#3325,#3326,#3327));
#908=EDGE_LOOP('',(#3328,#3329,#3330,#3331));
#909=EDGE_LOOP('',(#3332));
#910=EDGE_LOOP('',(#3333,#3334,#3335,#3336));
#911=EDGE_LOOP('',(#3337,#3338,#3339,#3340));
#912=EDGE_LOOP('',(#3341,#3342,#3343,#3344));
#913=EDGE_LOOP('',(#3345,#3346,#3347,#3348));
#914=EDGE_LOOP('',(#3349,#3350,#3351,#3352));
#915=EDGE_LOOP('',(#3353,#3354,#3355,#3356));
#916=EDGE_LOOP('',(#3357,#3358,#3359,#3360));
#917=EDGE_LOOP('',(#3361,#3362,#3363,#3364));
#918=EDGE_LOOP('',(#3365,#3366,#3367,#3368));
#919=EDGE_LOOP('',(#3369,#3370,#3371,#3372));
#920=EDGE_LOOP('',(#3373,#3374,#3375,#3376));
#921=EDGE_LOOP('',(#3377,#3378,#3379,#3380));
#922=EDGE_LOOP('',(#3381,#3382,#3383,#3384));
#923=EDGE_LOOP('',(#3385,#3386,#3387,#3388));
#924=EDGE_LOOP('',(#3389,#3390,#3391,#3392));
#925=EDGE_LOOP('',(#3393,#3394,#3395,#3396));
#926=EDGE_LOOP('',(#3397,#3398,#3399,#3400));
#927=EDGE_LOOP('',(#3401,#3402,#3403,#3404));
#928=EDGE_LOOP('',(#3405,#3406,#3407,#3408));
#929=EDGE_LOOP('',(#3409,#3410,#3411,#3412));
#930=EDGE_LOOP('',(#3413,#3414,#3415,#3416));
#931=EDGE_LOOP('',(#3417,#3418,#3419,#3420));
#932=EDGE_LOOP('',(#3421,#3422,#3423,#3424));
#933=EDGE_LOOP('',(#3425,#3426,#3427,#3428,#3429,#3430,#3431,#3432));
#934=EDGE_LOOP('',(#3433,#3434,#3435,#3436,#3437,#3438,#3439,#3440,#3441,
#3442,#3443,#3444,#3445,#3446,#3447,#3448,#3449,#3450,#3451,#3452,#3453,
#3454,#3455,#3456,#3457,#3458));
#935=EDGE_LOOP('',(#3459,#3460,#3461,#3462));
#936=EDGE_LOOP('',(#3463,#3464,#3465,#3466,#3467,#3468,#3469,#3470,#3471,
#3472,#3473,#3474,#3475,#3476,#3477,#3478,#3479,#3480,#3481,#3482,#3483,
#3484,#3485,#3486,#3487,#3488,#3489));
#937=EDGE_LOOP('',(#3490,#3491,#3492,#3493));
#938=EDGE_LOOP('',(#3494,#3495,#3496,#3497));
#939=EDGE_LOOP('',(#3498,#3499,#3500,#3501));
#940=EDGE_LOOP('',(#3502,#3503,#3504,#3505));
#941=EDGE_LOOP('',(#3506,#3507,#3508,#3509));
#942=EDGE_LOOP('',(#3510,#3511,#3512,#3513));
#943=EDGE_LOOP('',(#3514,#3515,#3516,#3517));
#944=EDGE_LOOP('',(#3518,#3519,#3520,#3521,#3522,#3523));
#945=EDGE_LOOP('',(#3524));
#946=EDGE_LOOP('',(#3525,#3526,#3527,#3528));
#947=EDGE_LOOP('',(#3529,#3530,#3531,#3532));
#948=EDGE_LOOP('',(#3533));
#949=EDGE_LOOP('',(#3534,#3535,#3536,#3537,#3538,#3539));
#950=EDGE_LOOP('',(#3540));
#951=LINE('',#5410,#1244);
#952=LINE('',#5413,#1245);
#953=LINE('',#5416,#1246);
#954=LINE('',#5418,#1247);
#955=LINE('',#5419,#1248);
#956=LINE('',#5422,#1249);
#957=LINE('',#5426,#1250);
#958=LINE('',#5430,#1251);
#959=LINE('',#5434,#1252);
#960=LINE('',#5438,#1253);
#961=LINE('',#5442,#1254);
#962=LINE('',#5446,#1255);
#963=LINE('',#5450,#1256);
#964=LINE('',#5453,#1257);
#965=LINE('',#5456,#1258);
#966=LINE('',#5457,#1259);
#967=LINE('',#5461,#1260);
#968=LINE('',#5464,#1261);
#969=LINE('',#5470,#1262);
#970=LINE('',#5471,#1263);
#971=LINE('',#5474,#1264);
#972=LINE('',#5475,#1265);
#973=LINE('',#5479,#1266);
#974=LINE('',#5482,#1267);
#975=LINE('',#5483,#1268);
#976=LINE('',#5487,#1269);
#977=LINE('',#5490,#1270);
#978=LINE('',#5491,#1271);
#979=LINE('',#5495,#1272);
#980=LINE('',#5497,#1273);
#981=LINE('',#5499,#1274);
#982=LINE('',#5501,#1275);
#983=LINE('',#5508,#1276);
#984=LINE('',#5514,#1277);
#985=LINE('',#5521,#1278);
#986=LINE('',#5524,#1279);
#987=LINE('',#5527,#1280);
#988=LINE('',#5529,#1281);
#989=LINE('',#5530,#1282);
#990=LINE('',#5533,#1283);
#991=LINE('',#5537,#1284);
#992=LINE('',#5541,#1285);
#993=LINE('',#5545,#1286);
#994=LINE('',#5549,#1287);
#995=LINE('',#5553,#1288);
#996=LINE('',#5557,#1289);
#997=LINE('',#5561,#1290);
#998=LINE('',#5564,#1291);
#999=LINE('',#5567,#1292);
#1000=LINE('',#5568,#1293);
#1001=LINE('',#5572,#1294);
#1002=LINE('',#5575,#1295);
#1003=LINE('',#5581,#1296);
#1004=LINE('',#5582,#1297);
#1005=LINE('',#5585,#1298);
#1006=LINE('',#5586,#1299);
#1007=LINE('',#5590,#1300);
#1008=LINE('',#5593,#1301);
#1009=LINE('',#5594,#1302);
#1010=LINE('',#5598,#1303);
#1011=LINE('',#5601,#1304);
#1012=LINE('',#5602,#1305);
#1013=LINE('',#5606,#1306);
#1014=LINE('',#5608,#1307);
#1015=LINE('',#5610,#1308);
#1016=LINE('',#5612,#1309);
#1017=LINE('',#5620,#1310);
#1018=LINE('',#5623,#1311);
#1019=LINE('',#5626,#1312);
#1020=LINE('',#5628,#1313);
#1021=LINE('',#5629,#1314);
#1022=LINE('',#5632,#1315);
#1023=LINE('',#5636,#1316);
#1024=LINE('',#5640,#1317);
#1025=LINE('',#5644,#1318);
#1026=LINE('',#5648,#1319);
#1027=LINE('',#5652,#1320);
#1028=LINE('',#5656,#1321);
#1029=LINE('',#5660,#1322);
#1030=LINE('',#5663,#1323);
#1031=LINE('',#5666,#1324);
#1032=LINE('',#5667,#1325);
#1033=LINE('',#5671,#1326);
#1034=LINE('',#5674,#1327);
#1035=LINE('',#5680,#1328);
#1036=LINE('',#5681,#1329);
#1037=LINE('',#5684,#1330);
#1038=LINE('',#5685,#1331);
#1039=LINE('',#5689,#1332);
#1040=LINE('',#5692,#1333);
#1041=LINE('',#5693,#1334);
#1042=LINE('',#5697,#1335);
#1043=LINE('',#5700,#1336);
#1044=LINE('',#5701,#1337);
#1045=LINE('',#5705,#1338);
#1046=LINE('',#5707,#1339);
#1047=LINE('',#5709,#1340);
#1048=LINE('',#5711,#1341);
#1049=LINE('',#5718,#1342);
#1050=LINE('',#5724,#1343);
#1051=LINE('',#5731,#1344);
#1052=LINE('',#5734,#1345);
#1053=LINE('',#5737,#1346);
#1054=LINE('',#5741,#1347);
#1055=LINE('',#5745,#1348);
#1056=LINE('',#5749,#1349);
#1057=LINE('',#5753,#1350);
#1058=LINE('',#5757,#1351);
#1059=LINE('',#5761,#1352);
#1060=LINE('',#5764,#1353);
#1061=LINE('',#5767,#1354);
#1062=LINE('',#5768,#1355);
#1063=LINE('',#5772,#1356);
#1064=LINE('',#5775,#1357);
#1065=LINE('',#5778,#1358);
#1066=LINE('',#5781,#1359);
#1067=LINE('',#5782,#1360);
#1068=LINE('',#5786,#1361);
#1069=LINE('',#5791,#1362);
#1070=LINE('',#5792,#1363);
#1071=LINE('',#5795,#1364);
#1072=LINE('',#5796,#1365);
#1073=LINE('',#5800,#1366);
#1074=LINE('',#5803,#1367);
#1075=LINE('',#5804,#1368);
#1076=LINE('',#5808,#1369);
#1077=LINE('',#5811,#1370);
#1078=LINE('',#5814,#1371);
#1079=LINE('',#5816,#1372);
#1080=LINE('',#5818,#1373);
#1081=LINE('',#5820,#1374);
#1082=LINE('',#5822,#1375);
#1083=LINE('',#5829,#1376);
#1084=LINE('',#5835,#1377);
#1085=LINE('',#5841,#1378);
#1086=LINE('',#5847,#1379);
#1087=LINE('',#5853,#1380);
#1088=LINE('',#5859,#1381);
#1089=LINE('',#5865,#1382);
#1090=LINE('',#5871,#1383);
#1091=LINE('',#5876,#1384);
#1092=LINE('',#5878,#1385);
#1093=LINE('',#5880,#1386);
#1094=LINE('',#5881,#1387);
#1095=LINE('',#5884,#1388);
#1096=LINE('',#5886,#1389);
#1097=LINE('',#5887,#1390);
#1098=LINE('',#5891,#1391);
#1099=LINE('',#5893,#1392);
#1100=LINE('',#5895,#1393);
#1101=LINE('',#5896,#1394);
#1102=LINE('',#5899,#1395);
#1103=LINE('',#5901,#1396);
#1104=LINE('',#5902,#1397);
#1105=LINE('',#5906,#1398);
#1106=LINE('',#5908,#1399);
#1107=LINE('',#5910,#1400);
#1108=LINE('',#5911,#1401);
#1109=LINE('',#5914,#1402);
#1110=LINE('',#5916,#1403);
#1111=LINE('',#5917,#1404);
#1112=LINE('',#5921,#1405);
#1113=LINE('',#5923,#1406);
#1114=LINE('',#5925,#1407);
#1115=LINE('',#5926,#1408);
#1116=LINE('',#5929,#1409);
#1117=LINE('',#5931,#1410);
#1118=LINE('',#5932,#1411);
#1119=LINE('',#5934,#1412);
#1120=LINE('',#5935,#1413);
#1121=LINE('',#5937,#1414);
#1122=LINE('',#5938,#1415);
#1123=LINE('',#5940,#1416);
#1124=LINE('',#5941,#1417);
#1125=LINE('',#5943,#1418);
#1126=LINE('',#5944,#1419);
#1127=LINE('',#5952,#1420);
#1128=LINE('',#5958,#1421);
#1129=LINE('',#5964,#1422);
#1130=LINE('',#5970,#1423);
#1131=LINE('',#5975,#1424);
#1132=LINE('',#5977,#1425);
#1133=LINE('',#5979,#1426);
#1134=LINE('',#5980,#1427);
#1135=LINE('',#5983,#1428);
#1136=LINE('',#5985,#1429);
#1137=LINE('',#5986,#1430);
#1138=LINE('',#5989,#1431);
#1139=LINE('',#5991,#1432);
#1140=LINE('',#5992,#1433);
#1141=LINE('',#5994,#1434);
#1142=LINE('',#5995,#1435);
#1143=LINE('',#6003,#1436);
#1144=LINE('',#6009,#1437);
#1145=LINE('',#6015,#1438);
#1146=LINE('',#6021,#1439);
#1147=LINE('',#6026,#1440);
#1148=LINE('',#6028,#1441);
#1149=LINE('',#6030,#1442);
#1150=LINE('',#6031,#1443);
#1151=LINE('',#6034,#1444);
#1152=LINE('',#6036,#1445);
#1153=LINE('',#6037,#1446);
#1154=LINE('',#6040,#1447);
#1155=LINE('',#6042,#1448);
#1156=LINE('',#6043,#1449);
#1157=LINE('',#6045,#1450);
#1158=LINE('',#6046,#1451);
#1159=LINE('',#6053,#1452);
#1160=LINE('',#6055,#1453);
#1161=LINE('',#6057,#1454);
#1162=LINE('',#6058,#1455);
#1163=LINE('',#6061,#1456);
#1164=LINE('',#6063,#1457);
#1165=LINE('',#6064,#1458);
#1166=LINE('',#6067,#1459);
#1167=LINE('',#6069,#1460);
#1168=LINE('',#6070,#1461);
#1169=LINE('',#6072,#1462);
#1170=LINE('',#6073,#1463);
#1171=LINE('',#6080,#1464);
#1172=LINE('',#6082,#1465);
#1173=LINE('',#6084,#1466);
#1174=LINE('',#6085,#1467);
#1175=LINE('',#6088,#1468);
#1176=LINE('',#6090,#1469);
#1177=LINE('',#6091,#1470);
#1178=LINE('',#6093,#1471);
#1179=LINE('',#6094,#1472);
#1180=LINE('',#6101,#1473);
#1181=LINE('',#6140,#1474);
#1182=LINE('',#6191,#1475);
#1183=LINE('',#6242,#1476);
#1184=LINE('',#6290,#1477);
#1185=LINE('',#6341,#1478);
#1186=LINE('',#6392,#1479);
#1187=LINE('',#6440,#1480);
#1188=LINE('',#6491,#1481);
#1189=LINE('',#6512,#1482);
#1190=LINE('',#6536,#1483);
#1191=LINE('',#6560,#1484);
#1192=LINE('',#6585,#1485);
#1193=LINE('',#6610,#1486);
#1194=LINE('',#6634,#1487);
#1195=LINE('',#6659,#1488);
#1196=LINE('',#6684,#1489);
#1197=LINE('',#6708,#1490);
#1198=LINE('',#7665,#1491);
#1199=LINE('',#7668,#1492);
#1200=LINE('',#7676,#1493);
#1201=LINE('',#7679,#1494);
#1202=LINE('',#7685,#1495);
#1203=LINE('',#7709,#1496);
#1204=LINE('',#7757,#1497);
#1205=LINE('',#7805,#1498);
#1206=LINE('',#7859,#1499);
#1207=LINE('',#7907,#1500);
#1208=LINE('',#7955,#1501);
#1209=LINE('',#8009,#1502);
#1210=LINE('',#8057,#1503);
#1211=LINE('',#8108,#1504);
#1212=LINE('',#8159,#1505);
#1213=LINE('',#8207,#1506);
#1214=LINE('',#8232,#1507);
#1215=LINE('',#8257,#1508);
#1216=LINE('',#8281,#1509);
#1217=LINE('',#8307,#1510);
#1218=LINE('',#8331,#1511);
#1219=LINE('',#8356,#1512);
#1220=LINE('',#8381,#1513);
#1221=LINE('',#8405,#1514);
#1222=LINE('',#8430,#1515);
#1223=LINE('',#8455,#1516);
#1224=LINE('',#8791,#1517);
#1225=LINE('',#9659,#1518);
#1226=LINE('',#9661,#1519);
#1227=LINE('',#9663,#1520);
#1228=LINE('',#9664,#1521);
#1229=LINE('',#9667,#1522);
#1230=LINE('',#9669,#1523);
#1231=LINE('',#9670,#1524);
#1232=LINE('',#9673,#1525);
#1233=LINE('',#9675,#1526);
#1234=LINE('',#9676,#1527);
#1235=LINE('',#9679,#1528);
#1236=LINE('',#9681,#1529);
#1237=LINE('',#9682,#1530);
#1238=LINE('',#9685,#1531);
#1239=LINE('',#9687,#1532);
#1240=LINE('',#9688,#1533);
#1241=LINE('',#9690,#1534);
#1242=LINE('',#9691,#1535);
#1243=LINE('',#9698,#1536);
#1244=VECTOR('',#4360,10.);
#1245=VECTOR('',#4363,10.);
#1246=VECTOR('',#4366,10.);
#1247=VECTOR('',#4367,10.);
#1248=VECTOR('',#4368,10.);
#1249=VECTOR('',#4371,10.);
#1250=VECTOR('',#4374,10.);
#1251=VECTOR('',#4377,10.);
#1252=VECTOR('',#4380,10.);
#1253=VECTOR('',#4383,10.);
#1254=VECTOR('',#4386,10.);
#1255=VECTOR('',#4389,10.);
#1256=VECTOR('',#4394,10.);
#1257=VECTOR('',#4397,10.);
#1258=VECTOR('',#4400,10.);
#1259=VECTOR('',#4401,10.);
#1260=VECTOR('',#4406,10.);
#1261=VECTOR('',#4409,10.);
#1262=VECTOR('',#4416,10.);
#1263=VECTOR('',#4417,10.);
#1264=VECTOR('',#4420,10.);
#1265=VECTOR('',#4421,10.);
#1266=VECTOR('',#4426,10.);
#1267=VECTOR('',#4429,10.);
#1268=VECTOR('',#4430,10.);
#1269=VECTOR('',#4435,10.);
#1270=VECTOR('',#4438,10.);
#1271=VECTOR('',#4439,10.);
#1272=VECTOR('',#4444,10.);
#1273=VECTOR('',#4447,10.);
#1274=VECTOR('',#4450,10.);
#1275=VECTOR('',#4453,10.);
#1276=VECTOR('',#4462,5.);
#1277=VECTOR('',#4469,5.);
#1278=VECTOR('',#4476,10.);
#1279=VECTOR('',#4479,10.);
#1280=VECTOR('',#4482,10.);
#1281=VECTOR('',#4483,10.);
#1282=VECTOR('',#4484,10.);
#1283=VECTOR('',#4487,10.);
#1284=VECTOR('',#4490,10.);
#1285=VECTOR('',#4493,10.);
#1286=VECTOR('',#4496,10.);
#1287=VECTOR('',#4499,10.);
#1288=VECTOR('',#4502,10.);
#1289=VECTOR('',#4505,10.);
#1290=VECTOR('',#4510,10.);
#1291=VECTOR('',#4513,10.);
#1292=VECTOR('',#4516,10.);
#1293=VECTOR('',#4517,10.);
#1294=VECTOR('',#4522,10.);
#1295=VECTOR('',#4525,10.);
#1296=VECTOR('',#4532,10.);
#1297=VECTOR('',#4533,10.);
#1298=VECTOR('',#4536,10.);
#1299=VECTOR('',#4537,10.);
#1300=VECTOR('',#4542,10.);
#1301=VECTOR('',#4545,10.);
#1302=VECTOR('',#4546,10.);
#1303=VECTOR('',#4551,10.);
#1304=VECTOR('',#4554,10.);
#1305=VECTOR('',#4555,10.);
#1306=VECTOR('',#4560,10.);
#1307=VECTOR('',#4563,10.);
#1308=VECTOR('',#4566,10.);
#1309=VECTOR('',#4569,10.);
#1310=VECTOR('',#4578,10.);
#1311=VECTOR('',#4581,10.);
#1312=VECTOR('',#4584,10.);
#1313=VECTOR('',#4585,10.);
#1314=VECTOR('',#4586,10.);
#1315=VECTOR('',#4589,10.);
#1316=VECTOR('',#4592,10.);
#1317=VECTOR('',#4595,10.);
#1318=VECTOR('',#4598,10.);
#1319=VECTOR('',#4601,10.);
#1320=VECTOR('',#4604,10.);
#1321=VECTOR('',#4607,10.);
#1322=VECTOR('',#4612,10.);
#1323=VECTOR('',#4615,10.);
#1324=VECTOR('',#4618,10.);
#1325=VECTOR('',#4619,10.);
#1326=VECTOR('',#4624,10.);
#1327=VECTOR('',#4627,10.);
#1328=VECTOR('',#4634,10.);
#1329=VECTOR('',#4635,10.);
#1330=VECTOR('',#4638,10.);
#1331=VECTOR('',#4639,10.);
#1332=VECTOR('',#4644,10.);
#1333=VECTOR('',#4647,10.);
#1334=VECTOR('',#4648,10.);
#1335=VECTOR('',#4653,10.);
#1336=VECTOR('',#4656,10.);
#1337=VECTOR('',#4657,10.);
#1338=VECTOR('',#4662,10.);
#1339=VECTOR('',#4665,10.);
#1340=VECTOR('',#4668,10.);
#1341=VECTOR('',#4671,10.);
#1342=VECTOR('',#4680,4.5);
#1343=VECTOR('',#4687,4.5);
#1344=VECTOR('',#4694,10.);
#1345=VECTOR('',#4697,10.);
#1346=VECTOR('',#4700,10.);
#1347=VECTOR('',#4703,10.);
#1348=VECTOR('',#4706,10.);
#1349=VECTOR('',#4709,10.);
#1350=VECTOR('',#4712,10.);
#1351=VECTOR('',#4715,10.);
#1352=VECTOR('',#4718,10.);
#1353=VECTOR('',#4721,10.);
#1354=VECTOR('',#4724,10.);
#1355=VECTOR('',#4725,10.);
#1356=VECTOR('',#4730,10.);
#1357=VECTOR('',#4733,10.);
#1358=VECTOR('',#4736,10.);
#1359=VECTOR('',#4739,10.);
#1360=VECTOR('',#4740,10.);
#1361=VECTOR('',#4745,10.);
#1362=VECTOR('',#4750,10.);
#1363=VECTOR('',#4751,10.);
#1364=VECTOR('',#4754,10.);
#1365=VECTOR('',#4755,10.);
#1366=VECTOR('',#4760,10.);
#1367=VECTOR('',#4763,10.);
#1368=VECTOR('',#4764,10.);
#1369=VECTOR('',#4769,10.);
#1370=VECTOR('',#4772,10.);
#1371=VECTOR('',#4775,10.);
#1372=VECTOR('',#4778,10.);
#1373=VECTOR('',#4781,10.);
#1374=VECTOR('',#4784,10.);
#1375=VECTOR('',#4787,10.);
#1376=VECTOR('',#4796,3.5);
#1377=VECTOR('',#4803,3.5);
#1378=VECTOR('',#4810,3.5);
#1379=VECTOR('',#4817,3.5);
#1380=VECTOR('',#4824,3.5);
#1381=VECTOR('',#4831,3.5);
#1382=VECTOR('',#4838,3.5);
#1383=VECTOR('',#4845,3.5);
#1384=VECTOR('',#4850,10.);
#1385=VECTOR('',#4851,10.);
#1386=VECTOR('',#4852,10.);
#1387=VECTOR('',#4853,10.);
#1388=VECTOR('',#4856,10.);
#1389=VECTOR('',#4857,10.);
#1390=VECTOR('',#4858,10.);
#1391=VECTOR('',#4861,10.);
#1392=VECTOR('',#4862,10.);
#1393=VECTOR('',#4863,10.);
#1394=VECTOR('',#4864,10.);
#1395=VECTOR('',#4867,10.);
#1396=VECTOR('',#4868,10.);
#1397=VECTOR('',#4869,10.);
#1398=VECTOR('',#4872,10.);
#1399=VECTOR('',#4873,10.);
#1400=VECTOR('',#4874,10.);
#1401=VECTOR('',#4875,10.);
#1402=VECTOR('',#4878,10.);
#1403=VECTOR('',#4879,10.);
#1404=VECTOR('',#4880,10.);
#1405=VECTOR('',#4883,10.);
#1406=VECTOR('',#4884,10.);
#1407=VECTOR('',#4885,10.);
#1408=VECTOR('',#4886,10.);
#1409=VECTOR('',#4889,10.);
#1410=VECTOR('',#4890,10.);
#1411=VECTOR('',#4891,10.);
#1412=VECTOR('',#4894,10.);
#1413=VECTOR('',#4895,10.);
#1414=VECTOR('',#4898,10.);
#1415=VECTOR('',#4899,10.);
#1416=VECTOR('',#4902,10.);
#1417=VECTOR('',#4903,10.);
#1418=VECTOR('',#4906,10.);
#1419=VECTOR('',#4907,10.);
#1420=VECTOR('',#4918,7.);
#1421=VECTOR('',#4925,7.);
#1422=VECTOR('',#4932,7.);
#1423=VECTOR('',#4939,7.);
#1424=VECTOR('',#4944,10.);
#1425=VECTOR('',#4945,10.);
#1426=VECTOR('',#4946,10.);
#1427=VECTOR('',#4947,10.);
#1428=VECTOR('',#4950,10.);
#1429=VECTOR('',#4951,10.);
#1430=VECTOR('',#4952,10.);
#1431=VECTOR('',#4955,10.);
#1432=VECTOR('',#4956,10.);
#1433=VECTOR('',#4957,10.);
#1434=VECTOR('',#4960,10.);
#1435=VECTOR('',#4961,10.);
#1436=VECTOR('',#4972,7.);
#1437=VECTOR('',#4979,7.);
#1438=VECTOR('',#4986,7.);
#1439=VECTOR('',#4993,7.);
#1440=VECTOR('',#4998,10.);
#1441=VECTOR('',#4999,10.);
#1442=VECTOR('',#5000,10.);
#1443=VECTOR('',#5001,10.);
#1444=VECTOR('',#5004,10.);
#1445=VECTOR('',#5005,10.);
#1446=VECTOR('',#5006,10.);
#1447=VECTOR('',#5009,10.);
#1448=VECTOR('',#5010,10.);
#1449=VECTOR('',#5011,10.);
#1450=VECTOR('',#5014,10.);
#1451=VECTOR('',#5015,10.);
#1452=VECTOR('',#5024,10.);
#1453=VECTOR('',#5025,10.);
#1454=VECTOR('',#5026,10.);
#1455=VECTOR('',#5027,10.);
#1456=VECTOR('',#5030,10.);
#1457=VECTOR('',#5031,10.);
#1458=VECTOR('',#5032,10.);
#1459=VECTOR('',#5035,10.);
#1460=VECTOR('',#5036,10.);
#1461=VECTOR('',#5037,10.);
#1462=VECTOR('',#5040,10.);
#1463=VECTOR('',#5041,10.);
#1464=VECTOR('',#5050,10.);
#1465=VECTOR('',#5051,10.);
#1466=VECTOR('',#5052,10.);
#1467=VECTOR('',#5053,10.);
#1468=VECTOR('',#5056,10.);
#1469=VECTOR('',#5057,10.);
#1470=VECTOR('',#5058,10.);
#1471=VECTOR('',#5061,10.);
#1472=VECTOR('',#5062,10.);
#1473=VECTOR('',#5071,3.);
#1474=VECTOR('',#5076,3.);
#1475=VECTOR('',#5079,3.);
#1476=VECTOR('',#5082,3.);
#1477=VECTOR('',#5085,3.);
#1478=VECTOR('',#5088,3.);
#1479=VECTOR('',#5091,3.);
#1480=VECTOR('',#5094,3.);
#1481=VECTOR('',#5097,3.);
#1482=VECTOR('',#5102,3.0735);
#1483=VECTOR('',#5107,3.0735);
#1484=VECTOR('',#5110,3.0735);
#1485=VECTOR('',#5113,3.0735);
#1486=VECTOR('',#5116,3.0735);
#1487=VECTOR('',#5119,3.0735);
#1488=VECTOR('',#5122,3.0735);
#1489=VECTOR('',#5125,3.0735);
#1490=VECTOR('',#5128,3.0735);
#1491=VECTOR('',#5151,7.);
#1492=VECTOR('',#5154,5.);
#1493=VECTOR('',#5165,7.);
#1494=VECTOR('',#5170,5.);
#1495=VECTOR('',#5177,3.);
#1496=VECTOR('',#5182,3.);
#1497=VECTOR('',#5185,3.);
#1498=VECTOR('',#5188,3.);
#1499=VECTOR('',#5191,3.);
#1500=VECTOR('',#5194,3.);
#1501=VECTOR('',#5197,3.);
#1502=VECTOR('',#5200,3.);
#1503=VECTOR('',#5203,3.);
#1504=VECTOR('',#5206,3.);
#1505=VECTOR('',#5209,3.);
#1506=VECTOR('',#5212,2.37175);
#1507=VECTOR('',#5217,2.37175);
#1508=VECTOR('',#5220,2.37175);
#1509=VECTOR('',#5223,2.37175);
#1510=VECTOR('',#5226,2.37175);
#1511=VECTOR('',#5229,2.37175);
#1512=VECTOR('',#5232,2.37175);
#1513=VECTOR('',#5235,2.37175);
#1514=VECTOR('',#5238,2.37175);
#1515=VECTOR('',#5241,2.37175);
#1516=VECTOR('',#5244,2.37175);
#1517=VECTOR('',#5249,2.5);
#1518=VECTOR('',#5260,10.);
#1519=VECTOR('',#5261,10.);
#1520=VECTOR('',#5262,10.);
#1521=VECTOR('',#5263,10.);
#1522=VECTOR('',#5266,10.);
#1523=VECTOR('',#5267,10.);
#1524=VECTOR('',#5268,10.);
#1525=VECTOR('',#5271,10.);
#1526=VECTOR('',#5272,10.);
#1527=VECTOR('',#5273,10.);
#1528=VECTOR('',#5276,10.);
#1529=VECTOR('',#5277,10.);
#1530=VECTOR('',#5278,10.);
#1531=VECTOR('',#5281,10.);
#1532=VECTOR('',#5282,10.);
#1533=VECTOR('',#5283,10.);
#1534=VECTOR('',#5286,10.);
#1535=VECTOR('',#5287,10.);
#1536=VECTOR('',#5296,5.);
#1537=CIRCLE('',#3976,1.);
#1538=CIRCLE('',#3977,1.);
#1539=CIRCLE('',#3980,1.);
#1540=CIRCLE('',#3981,1.);
#1541=CIRCLE('',#3982,1.);
#1542=CIRCLE('',#3983,1.);
#1543=CIRCLE('',#3984,1.);
#1544=CIRCLE('',#3985,1.);
#1545=CIRCLE('',#3986,1.);
#1546=CIRCLE('',#3988,1.);
#1547=CIRCLE('',#3991,1.);
#1548=CIRCLE('',#3993,1.);
#1549=CIRCLE('',#3995,1.);
#1550=CIRCLE('',#3998,1.);
#1551=CIRCLE('',#4001,1.);
#1552=CIRCLE('',#4004,1.);
#1553=CIRCLE('',#4011,5.);
#1554=CIRCLE('',#4012,5.);
#1555=CIRCLE('',#4014,5.);
#1556=CIRCLE('',#4015,5.);
#1557=CIRCLE('',#4017,1.);
#1558=CIRCLE('',#4018,1.);
#1559=CIRCLE('',#4021,1.);
#1560=CIRCLE('',#4022,1.);
#1561=CIRCLE('',#4023,1.);
#1562=CIRCLE('',#4024,1.);
#1563=CIRCLE('',#4025,1.);
#1564=CIRCLE('',#4026,1.);
#1565=CIRCLE('',#4027,1.);
#1566=CIRCLE('',#4029,1.);
#1567=CIRCLE('',#4032,1.);
#1568=CIRCLE('',#4034,1.);
#1569=CIRCLE('',#4036,1.);
#1570=CIRCLE('',#4039,1.);
#1571=CIRCLE('',#4042,1.);
#1572=CIRCLE('',#4045,1.);
#1573=CIRCLE('',#4052,1.);
#1574=CIRCLE('',#4053,1.);
#1575=CIRCLE('',#4056,1.);
#1576=CIRCLE('',#4057,1.);
#1577=CIRCLE('',#4058,1.);
#1578=CIRCLE('',#4059,1.);
#1579=CIRCLE('',#4060,1.);
#1580=CIRCLE('',#4061,1.);
#1581=CIRCLE('',#4062,1.);
#1582=CIRCLE('',#4064,1.);
#1583=CIRCLE('',#4067,1.);
#1584=CIRCLE('',#4069,1.);
#1585=CIRCLE('',#4071,1.);
#1586=CIRCLE('',#4074,1.);
#1587=CIRCLE('',#4077,1.);
#1588=CIRCLE('',#4080,1.);
#1589=CIRCLE('',#4087,4.5);
#1590=CIRCLE('',#4088,4.5);
#1591=CIRCLE('',#4090,4.5);
#1592=CIRCLE('',#4091,4.5);
#1593=CIRCLE('',#4093,1.);
#1594=CIRCLE('',#4094,1.);
#1595=CIRCLE('',#4096,1.);
#1596=CIRCLE('',#4097,1.);
#1597=CIRCLE('',#4098,1.);
#1598=CIRCLE('',#4099,1.);
#1599=CIRCLE('',#4100,1.);
#1600=CIRCLE('',#4101,1.);
#1601=CIRCLE('',#4102,1.);
#1602=CIRCLE('',#4105,1.);
#1603=CIRCLE('',#4107,1.);
#1604=CIRCLE('',#4110,1.);
#1605=CIRCLE('',#4112,1.);
#1606=CIRCLE('',#4115,1.);
#1607=CIRCLE('',#4118,1.);
#1608=CIRCLE('',#4120,1.);
#1609=CIRCLE('',#4128,3.5);
#1610=CIRCLE('',#4129,3.5);
#1611=CIRCLE('',#4131,3.5);
#1612=CIRCLE('',#4132,3.5);
#1613=CIRCLE('',#4134,3.5);
#1614=CIRCLE('',#4135,3.5);
#1615=CIRCLE('',#4137,3.5);
#1616=CIRCLE('',#4138,3.5);
#1617=CIRCLE('',#4140,3.5);
#1618=CIRCLE('',#4141,3.5);
#1619=CIRCLE('',#4143,3.5);
#1620=CIRCLE('',#4144,3.5);
#1621=CIRCLE('',#4146,3.5);
#1622=CIRCLE('',#4147,3.5);
#1623=CIRCLE('',#4149,3.5);
#1624=CIRCLE('',#4150,3.5);
#1625=CIRCLE('',#4167,7.);
#1626=CIRCLE('',#4168,7.);
#1627=CIRCLE('',#4170,7.);
#1628=CIRCLE('',#4171,7.);
#1629=CIRCLE('',#4173,7.);
#1630=CIRCLE('',#4174,7.);
#1631=CIRCLE('',#4176,7.);
#1632=CIRCLE('',#4177,7.);
#1633=CIRCLE('',#4186,7.);
#1634=CIRCLE('',#4187,7.);
#1635=CIRCLE('',#4189,7.);
#1636=CIRCLE('',#4190,7.);
#1637=CIRCLE('',#4192,7.);
#1638=CIRCLE('',#4193,7.);
#1639=CIRCLE('',#4195,7.);
#1640=CIRCLE('',#4196,7.);
#1641=CIRCLE('',#4218,2.5175);
#1642=CIRCLE('',#4227,2.5175);
#1643=CIRCLE('',#4229,3.0735);
#1644=CIRCLE('',#4238,3.0735);
#1645=CIRCLE('',#4241,7.);
#1646=CIRCLE('',#4243,7.);
#1647=CIRCLE('',#4244,5.);
#1648=CIRCLE('',#4246,7.);
#1649=CIRCLE('',#4247,5.);
#1650=CIRCLE('',#4250,5.);
#1651=CIRCLE('',#4252,7.);
#1652=CIRCLE('',#4253,5.);
#1653=CIRCLE('',#4260,2.942);
#1654=CIRCLE('',#4272,2.37175);
#1655=CIRCLE('',#4284,2.942);
#1656=CIRCLE('',#4285,2.);
#1657=CIRCLE('',#4287,2.37175);
#1658=CIRCLE('',#4297,5.);
#1659=CIRCLE('',#4299,5.);
#1660=VERTEX_POINT('',#5406);
#1661=VERTEX_POINT('',#5407);
#1662=VERTEX_POINT('',#5409);
#1663=VERTEX_POINT('',#5411);
#1664=VERTEX_POINT('',#5415);
#1665=VERTEX_POINT('',#5417);
#1666=VERTEX_POINT('',#5421);
#1667=VERTEX_POINT('',#5423);
#1668=VERTEX_POINT('',#5425);
#1669=VERTEX_POINT('',#5427);
#1670=VERTEX_POINT('',#5429);
#1671=VERTEX_POINT('',#5432);
#1672=VERTEX_POINT('',#5433);
#1673=VERTEX_POINT('',#5435);
#1674=VERTEX_POINT('',#5437);
#1675=VERTEX_POINT('',#5439);
#1676=VERTEX_POINT('',#5441);
#1677=VERTEX_POINT('',#5443);
#1678=VERTEX_POINT('',#5445);
#1679=VERTEX_POINT('',#5449);
#1680=VERTEX_POINT('',#5451);
#1681=VERTEX_POINT('',#5455);
#1682=VERTEX_POINT('',#5459);
#1683=VERTEX_POINT('',#5463);
#1684=VERTEX_POINT('',#5467);
#1685=VERTEX_POINT('',#5468);
#1686=VERTEX_POINT('',#5473);
#1687=VERTEX_POINT('',#5477);
#1688=VERTEX_POINT('',#5481);
#1689=VERTEX_POINT('',#5485);
#1690=VERTEX_POINT('',#5489);
#1691=VERTEX_POINT('',#5493);
#1692=VERTEX_POINT('',#5505);
#1693=VERTEX_POINT('',#5507);
#1694=VERTEX_POINT('',#5511);
#1695=VERTEX_POINT('',#5513);
#1696=VERTEX_POINT('',#5517);
#1697=VERTEX_POINT('',#5518);
#1698=VERTEX_POINT('',#5520);
#1699=VERTEX_POINT('',#5522);
#1700=VERTEX_POINT('',#5526);
#1701=VERTEX_POINT('',#5528);
#1702=VERTEX_POINT('',#5532);
#1703=VERTEX_POINT('',#5534);
#1704=VERTEX_POINT('',#5536);
#1705=VERTEX_POINT('',#5538);
#1706=VERTEX_POINT('',#5540);
#1707=VERTEX_POINT('',#5543);
#1708=VERTEX_POINT('',#5544);
#1709=VERTEX_POINT('',#5546);
#1710=VERTEX_POINT('',#5548);
#1711=VERTEX_POINT('',#5550);
#1712=VERTEX_POINT('',#5552);
#1713=VERTEX_POINT('',#5554);
#1714=VERTEX_POINT('',#5556);
#1715=VERTEX_POINT('',#5560);
#1716=VERTEX_POINT('',#5562);
#1717=VERTEX_POINT('',#5566);
#1718=VERTEX_POINT('',#5570);
#1719=VERTEX_POINT('',#5574);
#1720=VERTEX_POINT('',#5578);
#1721=VERTEX_POINT('',#5579);
#1722=VERTEX_POINT('',#5584);
#1723=VERTEX_POINT('',#5588);
#1724=VERTEX_POINT('',#5592);
#1725=VERTEX_POINT('',#5596);
#1726=VERTEX_POINT('',#5600);
#1727=VERTEX_POINT('',#5604);
#1728=VERTEX_POINT('',#5616);
#1729=VERTEX_POINT('',#5617);
#1730=VERTEX_POINT('',#5619);
#1731=VERTEX_POINT('',#5621);
#1732=VERTEX_POINT('',#5625);
#1733=VERTEX_POINT('',#5627);
#1734=VERTEX_POINT('',#5631);
#1735=VERTEX_POINT('',#5633);
#1736=VERTEX_POINT('',#5635);
#1737=VERTEX_POINT('',#5637);
#1738=VERTEX_POINT('',#5639);
#1739=VERTEX_POINT('',#5642);
#1740=VERTEX_POINT('',#5643);
#1741=VERTEX_POINT('',#5645);
#1742=VERTEX_POINT('',#5647);
#1743=VERTEX_POINT('',#5649);
#1744=VERTEX_POINT('',#5651);
#1745=VERTEX_POINT('',#5653);
#1746=VERTEX_POINT('',#5655);
#1747=VERTEX_POINT('',#5659);
#1748=VERTEX_POINT('',#5661);
#1749=VERTEX_POINT('',#5665);
#1750=VERTEX_POINT('',#5669);
#1751=VERTEX_POINT('',#5673);
#1752=VERTEX_POINT('',#5677);
#1753=VERTEX_POINT('',#5678);
#1754=VERTEX_POINT('',#5683);
#1755=VERTEX_POINT('',#5687);
#1756=VERTEX_POINT('',#5691);
#1757=VERTEX_POINT('',#5695);
#1758=VERTEX_POINT('',#5699);
#1759=VERTEX_POINT('',#5703);
#1760=VERTEX_POINT('',#5715);
#1761=VERTEX_POINT('',#5717);
#1762=VERTEX_POINT('',#5721);
#1763=VERTEX_POINT('',#5723);
#1764=VERTEX_POINT('',#5727);
#1765=VERTEX_POINT('',#5728);
#1766=VERTEX_POINT('',#5730);
#1767=VERTEX_POINT('',#5732);
#1768=VERTEX_POINT('',#5736);
#1769=VERTEX_POINT('',#5738);
#1770=VERTEX_POINT('',#5740);
#1771=VERTEX_POINT('',#5742);
#1772=VERTEX_POINT('',#5744);
#1773=VERTEX_POINT('',#5746);
#1774=VERTEX_POINT('',#5748);
#1775=VERTEX_POINT('',#5750);
#1776=VERTEX_POINT('',#5752);
#1777=VERTEX_POINT('',#5754);
#1778=VERTEX_POINT('',#5756);
#1779=VERTEX_POINT('',#5758);
#1780=VERTEX_POINT('',#5760);
#1781=VERTEX_POINT('',#5762);
#1782=VERTEX_POINT('',#5766);
#1783=VERTEX_POINT('',#5770);
#1784=VERTEX_POINT('',#5774);
#1785=VERTEX_POINT('',#5776);
#1786=VERTEX_POINT('',#5780);
#1787=VERTEX_POINT('',#5784);
#1788=VERTEX_POINT('',#5788);
#1789=VERTEX_POINT('',#5789);
#1790=VERTEX_POINT('',#5794);
#1791=VERTEX_POINT('',#5798);
#1792=VERTEX_POINT('',#5802);
#1793=VERTEX_POINT('',#5806);
#1794=VERTEX_POINT('',#5810);
#1795=VERTEX_POINT('',#5812);
#1796=VERTEX_POINT('',#5826);
#1797=VERTEX_POINT('',#5828);
#1798=VERTEX_POINT('',#5832);
#1799=VERTEX_POINT('',#5834);
#1800=VERTEX_POINT('',#5838);
#1801=VERTEX_POINT('',#5840);
#1802=VERTEX_POINT('',#5844);
#1803=VERTEX_POINT('',#5846);
#1804=VERTEX_POINT('',#5850);
#1805=VERTEX_POINT('',#5852);
#1806=VERTEX_POINT('',#5856);
#1807=VERTEX_POINT('',#5858);
#1808=VERTEX_POINT('',#5862);
#1809=VERTEX_POINT('',#5864);
#1810=VERTEX_POINT('',#5868);
#1811=VERTEX_POINT('',#5870);
#1812=VERTEX_POINT('',#5874);
#1813=VERTEX_POINT('',#5875);
#1814=VERTEX_POINT('',#5877);
#1815=VERTEX_POINT('',#5879);
#1816=VERTEX_POINT('',#5883);
#1817=VERTEX_POINT('',#5885);
#1818=VERTEX_POINT('',#5889);
#1819=VERTEX_POINT('',#5890);
#1820=VERTEX_POINT('',#5892);
#1821=VERTEX_POINT('',#5894);
#1822=VERTEX_POINT('',#5898);
#1823=VERTEX_POINT('',#5900);
#1824=VERTEX_POINT('',#5904);
#1825=VERTEX_POINT('',#5905);
#1826=VERTEX_POINT('',#5907);
#1827=VERTEX_POINT('',#5909);
#1828=VERTEX_POINT('',#5913);
#1829=VERTEX_POINT('',#5915);
#1830=VERTEX_POINT('',#5919);
#1831=VERTEX_POINT('',#5920);
#1832=VERTEX_POINT('',#5922);
#1833=VERTEX_POINT('',#5924);
#1834=VERTEX_POINT('',#5928);
#1835=VERTEX_POINT('',#5930);
#1836=VERTEX_POINT('',#5949);
#1837=VERTEX_POINT('',#5951);
#1838=VERTEX_POINT('',#5955);
#1839=VERTEX_POINT('',#5957);
#1840=VERTEX_POINT('',#5961);
#1841=VERTEX_POINT('',#5963);
#1842=VERTEX_POINT('',#5967);
#1843=VERTEX_POINT('',#5969);
#1844=VERTEX_POINT('',#5973);
#1845=VERTEX_POINT('',#5974);
#1846=VERTEX_POINT('',#5976);
#1847=VERTEX_POINT('',#5978);
#1848=VERTEX_POINT('',#5982);
#1849=VERTEX_POINT('',#5984);
#1850=VERTEX_POINT('',#5988);
#1851=VERTEX_POINT('',#5990);
#1852=VERTEX_POINT('',#6000);
#1853=VERTEX_POINT('',#6002);
#1854=VERTEX_POINT('',#6006);
#1855=VERTEX_POINT('',#6008);
#1856=VERTEX_POINT('',#6012);
#1857=VERTEX_POINT('',#6014);
#1858=VERTEX_POINT('',#6018);
#1859=VERTEX_POINT('',#6020);
#1860=VERTEX_POINT('',#6024);
#1861=VERTEX_POINT('',#6025);
#1862=VERTEX_POINT('',#6027);
#1863=VERTEX_POINT('',#6029);
#1864=VERTEX_POINT('',#6033);
#1865=VERTEX_POINT('',#6035);
#1866=VERTEX_POINT('',#6039);
#1867=VERTEX_POINT('',#6041);
#1868=VERTEX_POINT('',#6051);
#1869=VERTEX_POINT('',#6052);
#1870=VERTEX_POINT('',#6054);
#1871=VERTEX_POINT('',#6056);
#1872=VERTEX_POINT('',#6060);
#1873=VERTEX_POINT('',#6062);
#1874=VERTEX_POINT('',#6066);
#1875=VERTEX_POINT('',#6068);
#1876=VERTEX_POINT('',#6078);
#1877=VERTEX_POINT('',#6079);
#1878=VERTEX_POINT('',#6081);
#1879=VERTEX_POINT('',#6083);
#1880=VERTEX_POINT('',#6087);
#1881=VERTEX_POINT('',#6089);
#1882=VERTEX_POINT('',#6099);
#1883=VERTEX_POINT('',#6100);
#1884=VERTEX_POINT('',#6102);
#1885=VERTEX_POINT('',#6116);
#1886=VERTEX_POINT('',#6138);
#1887=VERTEX_POINT('',#6139);
#1888=VERTEX_POINT('',#6189);
#1889=VERTEX_POINT('',#6190);
#1890=VERTEX_POINT('',#6240);
#1891=VERTEX_POINT('',#6241);
#1892=VERTEX_POINT('',#6288);
#1893=VERTEX_POINT('',#6289);
#1894=VERTEX_POINT('',#6339);
#1895=VERTEX_POINT('',#6340);
#1896=VERTEX_POINT('',#6390);
#1897=VERTEX_POINT('',#6391);
#1898=VERTEX_POINT('',#6438);
#1899=VERTEX_POINT('',#6439);
#1900=VERTEX_POINT('',#6489);
#1901=VERTEX_POINT('',#6490);
#1902=VERTEX_POINT('',#6492);
#1903=VERTEX_POINT('',#6497);
#1904=VERTEX_POINT('',#6510);
#1905=VERTEX_POINT('',#6511);
#1906=VERTEX_POINT('',#6513);
#1907=VERTEX_POINT('',#6522);
#1908=VERTEX_POINT('',#6534);
#1909=VERTEX_POINT('',#6535);
#1910=VERTEX_POINT('',#6558);
#1911=VERTEX_POINT('',#6559);
#1912=VERTEX_POINT('',#6583);
#1913=VERTEX_POINT('',#6584);
#1914=VERTEX_POINT('',#6608);
#1915=VERTEX_POINT('',#6609);
#1916=VERTEX_POINT('',#6632);
#1917=VERTEX_POINT('',#6633);
#1918=VERTEX_POINT('',#6657);
#1919=VERTEX_POINT('',#6658);
#1920=VERTEX_POINT('',#6682);
#1921=VERTEX_POINT('',#6683);
#1922=VERTEX_POINT('',#6706);
#1923=VERTEX_POINT('',#6707);
#1924=VERTEX_POINT('',#6709);
#1925=VERTEX_POINT('',#6715);
#1926=VERTEX_POINT('',#7652);
#1927=VERTEX_POINT('',#7655);
#1928=VERTEX_POINT('',#7657);
#1929=VERTEX_POINT('',#7660);
#1930=VERTEX_POINT('',#7662);
#1931=VERTEX_POINT('',#7667);
#1932=VERTEX_POINT('',#7671);
#1933=VERTEX_POINT('',#7673);
#1934=VERTEX_POINT('',#7683);
#1935=VERTEX_POINT('',#7684);
#1936=VERTEX_POINT('',#7686);
#1937=VERTEX_POINT('',#7697);
#1938=VERTEX_POINT('',#7707);
#1939=VERTEX_POINT('',#7708);
#1940=VERTEX_POINT('',#7755);
#1941=VERTEX_POINT('',#7756);
#1942=VERTEX_POINT('',#7803);
#1943=VERTEX_POINT('',#7804);
#1944=VERTEX_POINT('',#7857);
#1945=VERTEX_POINT('',#7858);
#1946=VERTEX_POINT('',#7905);
#1947=VERTEX_POINT('',#7906);
#1948=VERTEX_POINT('',#7953);
#1949=VERTEX_POINT('',#7954);
#1950=VERTEX_POINT('',#8007);
#1951=VERTEX_POINT('',#8008);
#1952=VERTEX_POINT('',#8055);
#1953=VERTEX_POINT('',#8056);
#1954=VERTEX_POINT('',#8106);
#1955=VERTEX_POINT('',#8107);
#1956=VERTEX_POINT('',#8157);
#1957=VERTEX_POINT('',#8158);
#1958=VERTEX_POINT('',#8205);
#1959=VERTEX_POINT('',#8206);
#1960=VERTEX_POINT('',#8208);
#1961=VERTEX_POINT('',#8219);
#1962=VERTEX_POINT('',#8230);
#1963=VERTEX_POINT('',#8231);
#1964=VERTEX_POINT('',#8255);
#1965=VERTEX_POINT('',#8256);
#1966=VERTEX_POINT('',#8279);
#1967=VERTEX_POINT('',#8280);
#1968=VERTEX_POINT('',#8305);
#1969=VERTEX_POINT('',#8306);
#1970=VERTEX_POINT('',#8329);
#1971=VERTEX_POINT('',#8330);
#1972=VERTEX_POINT('',#8354);
#1973=VERTEX_POINT('',#8355);
#1974=VERTEX_POINT('',#8379);
#1975=VERTEX_POINT('',#8380);
#1976=VERTEX_POINT('',#8403);
#1977=VERTEX_POINT('',#8404);
#1978=VERTEX_POINT('',#8428);
#1979=VERTEX_POINT('',#8429);
#1980=VERTEX_POINT('',#8453);
#1981=VERTEX_POINT('',#8454);
#1982=VERTEX_POINT('',#8477);
#1983=VERTEX_POINT('',#8695);
#1984=VERTEX_POINT('',#8757);
#1985=VERTEX_POINT('',#8790);
#1986=VERTEX_POINT('',#9101);
#1987=VERTEX_POINT('',#9218);
#1988=VERTEX_POINT('',#9657);
#1989=VERTEX_POINT('',#9658);
#1990=VERTEX_POINT('',#9660);
#1991=VERTEX_POINT('',#9662);
#1992=VERTEX_POINT('',#9666);
#1993=VERTEX_POINT('',#9668);
#1994=VERTEX_POINT('',#9672);
#1995=VERTEX_POINT('',#9674);
#1996=VERTEX_POINT('',#9678);
#1997=VERTEX_POINT('',#9680);
#1998=VERTEX_POINT('',#9684);
#1999=VERTEX_POINT('',#9686);
#2000=VERTEX_POINT('',#9694);
#2001=VERTEX_POINT('',#9697);
#2002=EDGE_CURVE('',#1660,#1661,#1537,.T.);
#2003=EDGE_CURVE('',#1661,#1662,#951,.T.);
#2004=EDGE_CURVE('',#1662,#1663,#1538,.T.);
#2005=EDGE_CURVE('',#1663,#1660,#952,.T.);
#2006=EDGE_CURVE('',#1664,#1661,#953,.T.);
#2007=EDGE_CURVE('',#1665,#1664,#954,.T.);
#2008=EDGE_CURVE('',#1665,#1662,#955,.T.);
#2009=EDGE_CURVE('',#1660,#1666,#956,.T.);
#2010=EDGE_CURVE('',#1667,#1666,#1539,.T.);
#2011=EDGE_CURVE('',#1667,#1668,#957,.T.);
#2012=EDGE_CURVE('',#1669,#1668,#1540,.T.);
#2013=EDGE_CURVE('',#1669,#1670,#958,.T.);
#2014=EDGE_CURVE('',#1664,#1670,#1541,.T.);
#2015=EDGE_CURVE('',#1671,#1672,#959,.T.);
#2016=EDGE_CURVE('',#1673,#1672,#1542,.T.);
#2017=EDGE_CURVE('',#1673,#1674,#960,.T.);
#2018=EDGE_CURVE('',#1675,#1674,#1543,.T.);
#2019=EDGE_CURVE('',#1675,#1676,#961,.T.);
#2020=EDGE_CURVE('',#1677,#1676,#1544,.T.);
#2021=EDGE_CURVE('',#1677,#1678,#962,.T.);
#2022=EDGE_CURVE('',#1671,#1678,#1545,.T.);
#2023=EDGE_CURVE('',#1666,#1679,#963,.T.);
#2024=EDGE_CURVE('',#1679,#1680,#1546,.T.);
#2025=EDGE_CURVE('',#1680,#1667,#964,.T.);
#2026=EDGE_CURVE('',#1680,#1681,#965,.T.);
#2027=EDGE_CURVE('',#1668,#1681,#966,.T.);
#2028=EDGE_CURVE('',#1681,#1682,#1547,.T.);
#2029=EDGE_CURVE('',#1682,#1669,#967,.T.);
#2030=EDGE_CURVE('',#1670,#1683,#968,.T.);
#2031=EDGE_CURVE('',#1683,#1665,#1548,.T.);
#2032=EDGE_CURVE('',#1684,#1685,#1549,.T.);
#2033=EDGE_CURVE('',#1685,#1673,#969,.T.);
#2034=EDGE_CURVE('',#1672,#1684,#970,.T.);
#2035=EDGE_CURVE('',#1685,#1686,#971,.T.);
#2036=EDGE_CURVE('',#1674,#1686,#972,.T.);
#2037=EDGE_CURVE('',#1686,#1687,#1550,.T.);
#2038=EDGE_CURVE('',#1687,#1675,#973,.T.);
#2039=EDGE_CURVE('',#1687,#1688,#974,.T.);
#2040=EDGE_CURVE('',#1676,#1688,#975,.T.);
#2041=EDGE_CURVE('',#1688,#1689,#1551,.T.);
#2042=EDGE_CURVE('',#1689,#1677,#976,.T.);
#2043=EDGE_CURVE('',#1689,#1690,#977,.T.);
#2044=EDGE_CURVE('',#1678,#1690,#978,.T.);
#2045=EDGE_CURVE('',#1690,#1691,#1552,.T.);
#2046=EDGE_CURVE('',#1691,#1671,#979,.T.);
#2047=EDGE_CURVE('',#1691,#1684,#980,.T.);
#2048=EDGE_CURVE('',#1682,#1683,#981,.T.);
#2049=EDGE_CURVE('',#1663,#1679,#982,.T.);
#2050=EDGE_CURVE('',#1692,#1692,#1553,.T.);
#2051=EDGE_CURVE('',#1692,#1693,#983,.T.);
#2052=EDGE_CURVE('',#1693,#1693,#1554,.T.);
#2053=EDGE_CURVE('',#1694,#1694,#1555,.T.);
#2054=EDGE_CURVE('',#1694,#1695,#984,.T.);
#2055=EDGE_CURVE('',#1695,#1695,#1556,.T.);
#2056=EDGE_CURVE('',#1696,#1697,#1557,.T.);
#2057=EDGE_CURVE('',#1697,#1698,#985,.T.);
#2058=EDGE_CURVE('',#1698,#1699,#1558,.T.);
#2059=EDGE_CURVE('',#1699,#1696,#986,.T.);
#2060=EDGE_CURVE('',#1700,#1697,#987,.T.);
#2061=EDGE_CURVE('',#1701,#1700,#988,.T.);
#2062=EDGE_CURVE('',#1701,#1698,#989,.T.);
#2063=EDGE_CURVE('',#1696,#1702,#990,.T.);
#2064=EDGE_CURVE('',#1703,#1702,#1559,.T.);
#2065=EDGE_CURVE('',#1703,#1704,#991,.T.);
#2066=EDGE_CURVE('',#1705,#1704,#1560,.T.);
#2067=EDGE_CURVE('',#1705,#1706,#992,.T.);
#2068=EDGE_CURVE('',#1700,#1706,#1561,.T.);
#2069=EDGE_CURVE('',#1707,#1708,#993,.T.);
#2070=EDGE_CURVE('',#1709,#1708,#1562,.T.);
#2071=EDGE_CURVE('',#1709,#1710,#994,.T.);
#2072=EDGE_CURVE('',#1711,#1710,#1563,.T.);
#2073=EDGE_CURVE('',#1711,#1712,#995,.T.);
#2074=EDGE_CURVE('',#1713,#1712,#1564,.T.);
#2075=EDGE_CURVE('',#1713,#1714,#996,.T.);
#2076=EDGE_CURVE('',#1707,#1714,#1565,.T.);
#2077=EDGE_CURVE('',#1702,#1715,#997,.T.);
#2078=EDGE_CURVE('',#1715,#1716,#1566,.T.);
#2079=EDGE_CURVE('',#1716,#1703,#998,.T.);
#2080=EDGE_CURVE('',#1716,#1717,#999,.T.);
#2081=EDGE_CURVE('',#1704,#1717,#1000,.T.);
#2082=EDGE_CURVE('',#1717,#1718,#1567,.T.);
#2083=EDGE_CURVE('',#1718,#1705,#1001,.T.);
#2084=EDGE_CURVE('',#1706,#1719,#1002,.T.);
#2085=EDGE_CURVE('',#1719,#1701,#1568,.T.);
#2086=EDGE_CURVE('',#1720,#1721,#1569,.T.);
#2087=EDGE_CURVE('',#1721,#1709,#1003,.T.);
#2088=EDGE_CURVE('',#1708,#1720,#1004,.T.);
#2089=EDGE_CURVE('',#1721,#1722,#1005,.T.);
#2090=EDGE_CURVE('',#1710,#1722,#1006,.T.);
#2091=EDGE_CURVE('',#1722,#1723,#1570,.T.);
#2092=EDGE_CURVE('',#1723,#1711,#1007,.T.);
#2093=EDGE_CURVE('',#1723,#1724,#1008,.T.);
#2094=EDGE_CURVE('',#1712,#1724,#1009,.T.);
#2095=EDGE_CURVE('',#1724,#1725,#1571,.T.);
#2096=EDGE_CURVE('',#1725,#1713,#1010,.T.);
#2097=EDGE_CURVE('',#1725,#1726,#1011,.T.);
#2098=EDGE_CURVE('',#1714,#1726,#1012,.T.);
#2099=EDGE_CURVE('',#1726,#1727,#1572,.T.);
#2100=EDGE_CURVE('',#1727,#1707,#1013,.T.);
#2101=EDGE_CURVE('',#1727,#1720,#1014,.T.);
#2102=EDGE_CURVE('',#1718,#1719,#1015,.T.);
#2103=EDGE_CURVE('',#1699,#1715,#1016,.T.);
#2104=EDGE_CURVE('',#1728,#1729,#1573,.T.);
#2105=EDGE_CURVE('',#1729,#1730,#1017,.T.);
#2106=EDGE_CURVE('',#1730,#1731,#1574,.T.);
#2107=EDGE_CURVE('',#1731,#1728,#1018,.T.);
#2108=EDGE_CURVE('',#1732,#1729,#1019,.T.);
#2109=EDGE_CURVE('',#1733,#1732,#1020,.T.);
#2110=EDGE_CURVE('',#1733,#1730,#1021,.T.);
#2111=EDGE_CURVE('',#1728,#1734,#1022,.T.);
#2112=EDGE_CURVE('',#1735,#1734,#1575,.T.);
#2113=EDGE_CURVE('',#1735,#1736,#1023,.T.);
#2114=EDGE_CURVE('',#1737,#1736,#1576,.T.);
#2115=EDGE_CURVE('',#1737,#1738,#1024,.T.);
#2116=EDGE_CURVE('',#1732,#1738,#1577,.T.);
#2117=EDGE_CURVE('',#1739,#1740,#1025,.T.);
#2118=EDGE_CURVE('',#1741,#1740,#1578,.T.);
#2119=EDGE_CURVE('',#1741,#1742,#1026,.T.);
#2120=EDGE_CURVE('',#1743,#1742,#1579,.T.);
#2121=EDGE_CURVE('',#1743,#1744,#1027,.T.);
#2122=EDGE_CURVE('',#1745,#1744,#1580,.T.);
#2123=EDGE_CURVE('',#1745,#1746,#1028,.T.);
#2124=EDGE_CURVE('',#1739,#1746,#1581,.T.);
#2125=EDGE_CURVE('',#1734,#1747,#1029,.T.);
#2126=EDGE_CURVE('',#1747,#1748,#1582,.T.);
#2127=EDGE_CURVE('',#1748,#1735,#1030,.T.);
#2128=EDGE_CURVE('',#1748,#1749,#1031,.T.);
#2129=EDGE_CURVE('',#1736,#1749,#1032,.T.);
#2130=EDGE_CURVE('',#1749,#1750,#1583,.T.);
#2131=EDGE_CURVE('',#1750,#1737,#1033,.T.);
#2132=EDGE_CURVE('',#1738,#1751,#1034,.T.);
#2133=EDGE_CURVE('',#1751,#1733,#1584,.T.);
#2134=EDGE_CURVE('',#1752,#1753,#1585,.T.);
#2135=EDGE_CURVE('',#1753,#1741,#1035,.T.);
#2136=EDGE_CURVE('',#1740,#1752,#1036,.T.);
#2137=EDGE_CURVE('',#1753,#1754,#1037,.T.);
#2138=EDGE_CURVE('',#1742,#1754,#1038,.T.);
#2139=EDGE_CURVE('',#1754,#1755,#1586,.T.);
#2140=EDGE_CURVE('',#1755,#1743,#1039,.T.);
#2141=EDGE_CURVE('',#1755,#1756,#1040,.T.);
#2142=EDGE_CURVE('',#1744,#1756,#1041,.T.);
#2143=EDGE_CURVE('',#1756,#1757,#1587,.T.);
#2144=EDGE_CURVE('',#1757,#1745,#1042,.T.);
#2145=EDGE_CURVE('',#1757,#1758,#1043,.T.);
#2146=EDGE_CURVE('',#1746,#1758,#1044,.T.);
#2147=EDGE_CURVE('',#1758,#1759,#1588,.T.);
#2148=EDGE_CURVE('',#1759,#1739,#1045,.T.);
#2149=EDGE_CURVE('',#1759,#1752,#1046,.T.);
#2150=EDGE_CURVE('',#1750,#1751,#1047,.T.);
#2151=EDGE_CURVE('',#1731,#1747,#1048,.T.);
#2152=EDGE_CURVE('',#1760,#1760,#1589,.T.);
#2153=EDGE_CURVE('',#1760,#1761,#1049,.T.);
#2154=EDGE_CURVE('',#1761,#1761,#1590,.T.);
#2155=EDGE_CURVE('',#1762,#1762,#1591,.T.);
#2156=EDGE_CURVE('',#1762,#1763,#1050,.T.);
#2157=EDGE_CURVE('',#1763,#1763,#1592,.T.);
#2158=EDGE_CURVE('',#1764,#1765,#1593,.T.);
#2159=EDGE_CURVE('',#1765,#1766,#1051,.T.);
#2160=EDGE_CURVE('',#1766,#1767,#1594,.T.);
#2161=EDGE_CURVE('',#1767,#1764,#1052,.T.);
#2162=EDGE_CURVE('',#1764,#1768,#1053,.T.);
#2163=EDGE_CURVE('',#1769,#1768,#1595,.T.);
#2164=EDGE_CURVE('',#1769,#1770,#1054,.T.);
#2165=EDGE_CURVE('',#1771,#1770,#1596,.T.);
#2166=EDGE_CURVE('',#1771,#1772,#1055,.T.);
#2167=EDGE_CURVE('',#1773,#1772,#1597,.T.);
#2168=EDGE_CURVE('',#1773,#1774,#1056,.T.);
#2169=EDGE_CURVE('',#1775,#1774,#1598,.T.);
#2170=EDGE_CURVE('',#1775,#1776,#1057,.T.);
#2171=EDGE_CURVE('',#1777,#1776,#1599,.T.);
#2172=EDGE_CURVE('',#1777,#1778,#1058,.T.);
#2173=EDGE_CURVE('',#1779,#1778,#1600,.T.);
#2174=EDGE_CURVE('',#1779,#1780,#1059,.T.);
#2175=EDGE_CURVE('',#1781,#1780,#1601,.T.);
#2176=EDGE_CURVE('',#1781,#1765,#1060,.T.);
#2177=EDGE_CURVE('',#1767,#1782,#1061,.T.);
#2178=EDGE_CURVE('',#1768,#1782,#1062,.T.);
#2179=EDGE_CURVE('',#1782,#1783,#1602,.T.);
#2180=EDGE_CURVE('',#1783,#1769,#1063,.T.);
#2181=EDGE_CURVE('',#1770,#1784,#1064,.T.);
#2182=EDGE_CURVE('',#1784,#1785,#1603,.T.);
#2183=EDGE_CURVE('',#1785,#1771,#1065,.T.);
#2184=EDGE_CURVE('',#1785,#1786,#1066,.T.);
#2185=EDGE_CURVE('',#1772,#1786,#1067,.T.);
#2186=EDGE_CURVE('',#1786,#1787,#1604,.T.);
#2187=EDGE_CURVE('',#1787,#1773,#1068,.T.);
#2188=EDGE_CURVE('',#1788,#1789,#1605,.T.);
#2189=EDGE_CURVE('',#1789,#1775,#1069,.T.);
#2190=EDGE_CURVE('',#1774,#1788,#1070,.T.);
#2191=EDGE_CURVE('',#1789,#1790,#1071,.T.);
#2192=EDGE_CURVE('',#1776,#1790,#1072,.T.);
#2193=EDGE_CURVE('',#1790,#1791,#1606,.T.);
#2194=EDGE_CURVE('',#1791,#1777,#1073,.T.);
#2195=EDGE_CURVE('',#1791,#1792,#1074,.T.);
#2196=EDGE_CURVE('',#1778,#1792,#1075,.T.);
#2197=EDGE_CURVE('',#1792,#1793,#1607,.T.);
#2198=EDGE_CURVE('',#1793,#1779,#1076,.T.);
#2199=EDGE_CURVE('',#1780,#1794,#1077,.T.);
#2200=EDGE_CURVE('',#1794,#1795,#1608,.T.);
#2201=EDGE_CURVE('',#1795,#1781,#1078,.T.);
#2202=EDGE_CURVE('',#1795,#1766,#1079,.T.);
#2203=EDGE_CURVE('',#1793,#1794,#1080,.T.);
#2204=EDGE_CURVE('',#1787,#1788,#1081,.T.);
#2205=EDGE_CURVE('',#1783,#1784,#1082,.T.);
#2206=EDGE_CURVE('',#1796,#1796,#1609,.T.);
#2207=EDGE_CURVE('',#1796,#1797,#1083,.T.);
#2208=EDGE_CURVE('',#1797,#1797,#1610,.T.);
#2209=EDGE_CURVE('',#1798,#1798,#1611,.T.);
#2210=EDGE_CURVE('',#1798,#1799,#1084,.T.);
#2211=EDGE_CURVE('',#1799,#1799,#1612,.T.);
#2212=EDGE_CURVE('',#1800,#1800,#1613,.T.);
#2213=EDGE_CURVE('',#1800,#1801,#1085,.T.);
#2214=EDGE_CURVE('',#1801,#1801,#1614,.T.);
#2215=EDGE_CURVE('',#1802,#1802,#1615,.T.);
#2216=EDGE_CURVE('',#1802,#1803,#1086,.T.);
#2217=EDGE_CURVE('',#1803,#1803,#1616,.T.);
#2218=EDGE_CURVE('',#1804,#1804,#1617,.T.);
#2219=EDGE_CURVE('',#1804,#1805,#1087,.T.);
#2220=EDGE_CURVE('',#1805,#1805,#1618,.T.);
#2221=EDGE_CURVE('',#1806,#1806,#1619,.T.);
#2222=EDGE_CURVE('',#1806,#1807,#1088,.T.);
#2223=EDGE_CURVE('',#1807,#1807,#1620,.T.);
#2224=EDGE_CURVE('',#1808,#1808,#1621,.T.);
#2225=EDGE_CURVE('',#1808,#1809,#1089,.T.);
#2226=EDGE_CURVE('',#1809,#1809,#1622,.T.);
#2227=EDGE_CURVE('',#1810,#1810,#1623,.T.);
#2228=EDGE_CURVE('',#1810,#1811,#1090,.T.);
#2229=EDGE_CURVE('',#1811,#1811,#1624,.T.);
#2230=EDGE_CURVE('',#1812,#1813,#1091,.T.);
#2231=EDGE_CURVE('',#1812,#1814,#1092,.T.);
#2232=EDGE_CURVE('',#1815,#1814,#1093,.T.);
#2233=EDGE_CURVE('',#1813,#1815,#1094,.T.);
#2234=EDGE_CURVE('',#1816,#1812,#1095,.T.);
#2235=EDGE_CURVE('',#1817,#1816,#1096,.T.);
#2236=EDGE_CURVE('',#1814,#1817,#1097,.T.);
#2237=EDGE_CURVE('',#1818,#1819,#1098,.T.);
#2238=EDGE_CURVE('',#1818,#1820,#1099,.T.);
#2239=EDGE_CURVE('',#1821,#1820,#1100,.T.);
#2240=EDGE_CURVE('',#1819,#1821,#1101,.T.);
#2241=EDGE_CURVE('',#1822,#1818,#1102,.T.);
#2242=EDGE_CURVE('',#1823,#1822,#1103,.T.);
#2243=EDGE_CURVE('',#1820,#1823,#1104,.T.);
#2244=EDGE_CURVE('',#1824,#1825,#1105,.T.);
#2245=EDGE_CURVE('',#1824,#1826,#1106,.T.);
#2246=EDGE_CURVE('',#1827,#1826,#1107,.T.);
#2247=EDGE_CURVE('',#1825,#1827,#1108,.T.);
#2248=EDGE_CURVE('',#1828,#1824,#1109,.T.);
#2249=EDGE_CURVE('',#1829,#1828,#1110,.T.);
#2250=EDGE_CURVE('',#1826,#1829,#1111,.T.);
#2251=EDGE_CURVE('',#1830,#1831,#1112,.T.);
#2252=EDGE_CURVE('',#1832,#1830,#1113,.T.);
#2253=EDGE_CURVE('',#1833,#1832,#1114,.T.);
#2254=EDGE_CURVE('',#1831,#1833,#1115,.T.);
#2255=EDGE_CURVE('',#1831,#1834,#1116,.T.);
#2256=EDGE_CURVE('',#1835,#1833,#1117,.T.);
#2257=EDGE_CURVE('',#1834,#1835,#1118,.T.);
#2258=EDGE_CURVE('',#1821,#1829,#1119,.T.);
#2259=EDGE_CURVE('',#1819,#1828,#1120,.T.);
#2260=EDGE_CURVE('',#1834,#1822,#1121,.T.);
#2261=EDGE_CURVE('',#1835,#1823,#1122,.T.);
#2262=EDGE_CURVE('',#1827,#1817,#1123,.T.);
#2263=EDGE_CURVE('',#1815,#1832,#1124,.T.);
#2264=EDGE_CURVE('',#1813,#1830,#1125,.T.);
#2265=EDGE_CURVE('',#1825,#1816,#1126,.T.);
#2266=EDGE_CURVE('',#1836,#1836,#1625,.T.);
#2267=EDGE_CURVE('',#1836,#1837,#1127,.T.);
#2268=EDGE_CURVE('',#1837,#1837,#1626,.T.);
#2269=EDGE_CURVE('',#1838,#1838,#1627,.T.);
#2270=EDGE_CURVE('',#1838,#1839,#1128,.T.);
#2271=EDGE_CURVE('',#1839,#1839,#1628,.T.);
#2272=EDGE_CURVE('',#1840,#1840,#1629,.T.);
#2273=EDGE_CURVE('',#1840,#1841,#1129,.T.);
#2274=EDGE_CURVE('',#1841,#1841,#1630,.T.);
#2275=EDGE_CURVE('',#1842,#1842,#1631,.T.);
#2276=EDGE_CURVE('',#1842,#1843,#1130,.T.);
#2277=EDGE_CURVE('',#1843,#1843,#1632,.T.);
#2278=EDGE_CURVE('',#1844,#1845,#1131,.T.);
#2279=EDGE_CURVE('',#1845,#1846,#1132,.T.);
#2280=EDGE_CURVE('',#1847,#1846,#1133,.T.);
#2281=EDGE_CURVE('',#1844,#1847,#1134,.T.);
#2282=EDGE_CURVE('',#1848,#1844,#1135,.T.);
#2283=EDGE_CURVE('',#1849,#1847,#1136,.T.);
#2284=EDGE_CURVE('',#1848,#1849,#1137,.T.);
#2285=EDGE_CURVE('',#1850,#1848,#1138,.T.);
#2286=EDGE_CURVE('',#1851,#1849,#1139,.T.);
#2287=EDGE_CURVE('',#1850,#1851,#1140,.T.);
#2288=EDGE_CURVE('',#1845,#1850,#1141,.T.);
#2289=EDGE_CURVE('',#1846,#1851,#1142,.T.);
#2290=EDGE_CURVE('',#1852,#1852,#1633,.T.);
#2291=EDGE_CURVE('',#1852,#1853,#1143,.T.);
#2292=EDGE_CURVE('',#1853,#1853,#1634,.T.);
#2293=EDGE_CURVE('',#1854,#1854,#1635,.T.);
#2294=EDGE_CURVE('',#1854,#1855,#1144,.T.);
#2295=EDGE_CURVE('',#1855,#1855,#1636,.T.);
#2296=EDGE_CURVE('',#1856,#1856,#1637,.T.);
#2297=EDGE_CURVE('',#1856,#1857,#1145,.T.);
#2298=EDGE_CURVE('',#1857,#1857,#1638,.T.);
#2299=EDGE_CURVE('',#1858,#1858,#1639,.T.);
#2300=EDGE_CURVE('',#1858,#1859,#1146,.T.);
#2301=EDGE_CURVE('',#1859,#1859,#1640,.T.);
#2302=EDGE_CURVE('',#1860,#1861,#1147,.T.);
#2303=EDGE_CURVE('',#1861,#1862,#1148,.T.);
#2304=EDGE_CURVE('',#1863,#1862,#1149,.T.);
#2305=EDGE_CURVE('',#1860,#1863,#1150,.T.);
#2306=EDGE_CURVE('',#1864,#1860,#1151,.T.);
#2307=EDGE_CURVE('',#1865,#1863,#1152,.T.);
#2308=EDGE_CURVE('',#1864,#1865,#1153,.T.);
#2309=EDGE_CURVE('',#1866,#1864,#1154,.T.);
#2310=EDGE_CURVE('',#1867,#1865,#1155,.T.);
#2311=EDGE_CURVE('',#1866,#1867,#1156,.T.);
#2312=EDGE_CURVE('',#1861,#1866,#1157,.T.);
#2313=EDGE_CURVE('',#1862,#1867,#1158,.T.);
#2314=EDGE_CURVE('',#1868,#1869,#1159,.T.);
#2315=EDGE_CURVE('',#1869,#1870,#1160,.T.);
#2316=EDGE_CURVE('',#1871,#1870,#1161,.T.);
#2317=EDGE_CURVE('',#1868,#1871,#1162,.T.);
#2318=EDGE_CURVE('',#1872,#1868,#1163,.T.);
#2319=EDGE_CURVE('',#1873,#1871,#1164,.T.);
#2320=EDGE_CURVE('',#1872,#1873,#1165,.T.);
#2321=EDGE_CURVE('',#1874,#1872,#1166,.T.);
#2322=EDGE_CURVE('',#1875,#1873,#1167,.T.);
#2323=EDGE_CURVE('',#1874,#1875,#1168,.T.);
#2324=EDGE_CURVE('',#1869,#1874,#1169,.T.);
#2325=EDGE_CURVE('',#1870,#1875,#1170,.T.);
#2326=EDGE_CURVE('',#1876,#1877,#1171,.T.);
#2327=EDGE_CURVE('',#1877,#1878,#1172,.T.);
#2328=EDGE_CURVE('',#1879,#1878,#1173,.T.);
#2329=EDGE_CURVE('',#1876,#1879,#1174,.T.);
#2330=EDGE_CURVE('',#1880,#1876,#1175,.T.);
#2331=EDGE_CURVE('',#1881,#1879,#1176,.T.);
#2332=EDGE_CURVE('',#1880,#1881,#1177,.T.);
#2333=EDGE_CURVE('',#1877,#1880,#1178,.T.);
#2334=EDGE_CURVE('',#1878,#1881,#1179,.T.);
#2335=EDGE_CURVE('',#1882,#1883,#1180,.T.);
#2336=EDGE_CURVE('',#1883,#1884,#216,.T.);
#2337=EDGE_CURVE('',#1884,#1885,#1641,.F.);
#2338=EDGE_CURVE('',#1885,#1882,#217,.T.);
#2339=EDGE_CURVE('',#1886,#1887,#1181,.T.);
#2340=EDGE_CURVE('',#1887,#1883,#218,.T.);
#2341=EDGE_CURVE('',#1882,#1886,#219,.T.);
#2342=EDGE_CURVE('',#1888,#1889,#1182,.T.);
#2343=EDGE_CURVE('',#1889,#1887,#220,.T.);
#2344=EDGE_CURVE('',#1886,#1888,#221,.T.);
#2345=EDGE_CURVE('',#1890,#1891,#1183,.T.);
#2346=EDGE_CURVE('',#1891,#1889,#222,.T.);
#2347=EDGE_CURVE('',#1888,#1890,#223,.T.);
#2348=EDGE_CURVE('',#1892,#1893,#1184,.T.);
#2349=EDGE_CURVE('',#1893,#1891,#224,.T.);
#2350=EDGE_CURVE('',#1890,#1892,#225,.T.);
#2351=EDGE_CURVE('',#1894,#1895,#1185,.T.);
#2352=EDGE_CURVE('',#1895,#1893,#226,.T.);
#2353=EDGE_CURVE('',#1892,#1894,#227,.T.);
#2354=EDGE_CURVE('',#1896,#1897,#1186,.T.);
#2355=EDGE_CURVE('',#1897,#1895,#228,.T.);
#2356=EDGE_CURVE('',#1894,#1896,#229,.T.);
#2357=EDGE_CURVE('',#1898,#1899,#1187,.T.);
#2358=EDGE_CURVE('',#1899,#1897,#230,.T.);
#2359=EDGE_CURVE('',#1896,#1898,#231,.T.);
#2360=EDGE_CURVE('',#1900,#1901,#1188,.T.);
#2361=EDGE_CURVE('',#1900,#1902,#232,.T.);
#2362=EDGE_CURVE('',#1903,#1902,#1642,.F.);
#2363=EDGE_CURVE('',#1903,#1901,#233,.T.);
#2364=EDGE_CURVE('',#1904,#1905,#1189,.T.);
#2365=EDGE_CURVE('',#1905,#1906,#234,.T.);
#2366=EDGE_CURVE('',#1907,#1906,#1643,.T.);
#2367=EDGE_CURVE('',#1904,#1907,#235,.T.);
#2368=EDGE_CURVE('',#1908,#1909,#1190,.T.);
#2369=EDGE_CURVE('',#1909,#1905,#236,.T.);
#2370=EDGE_CURVE('',#1908,#1904,#237,.T.);
#2371=EDGE_CURVE('',#1910,#1911,#1191,.T.);
#2372=EDGE_CURVE('',#1911,#1909,#238,.T.);
#2373=EDGE_CURVE('',#1910,#1908,#239,.T.);
#2374=EDGE_CURVE('',#1912,#1913,#1192,.T.);
#2375=EDGE_CURVE('',#1913,#1911,#240,.T.);
#2376=EDGE_CURVE('',#1912,#1910,#241,.T.);
#2377=EDGE_CURVE('',#1914,#1915,#1193,.T.);
#2378=EDGE_CURVE('',#1915,#1913,#242,.T.);
#2379=EDGE_CURVE('',#1914,#1912,#243,.T.);
#2380=EDGE_CURVE('',#1916,#1917,#1194,.T.);
#2381=EDGE_CURVE('',#1917,#1915,#244,.T.);
#2382=EDGE_CURVE('',#1916,#1914,#245,.T.);
#2383=EDGE_CURVE('',#1918,#1919,#1195,.T.);
#2384=EDGE_CURVE('',#1919,#1917,#246,.T.);
#2385=EDGE_CURVE('',#1918,#1916,#247,.T.);
#2386=EDGE_CURVE('',#1920,#1921,#1196,.T.);
#2387=EDGE_CURVE('',#1921,#1919,#248,.T.);
#2388=EDGE_CURVE('',#1920,#1918,#249,.T.);
#2389=EDGE_CURVE('',#1922,#1923,#1197,.T.);
#2390=EDGE_CURVE('',#1924,#1922,#250,.T.);
#2391=EDGE_CURVE('',#1925,#1924,#1644,.T.);
#2392=EDGE_CURVE('',#1925,#1923,#251,.T.);
#2393=EDGE_CURVE('',#1923,#1921,#252,.T.);
#2394=EDGE_CURVE('',#1922,#1920,#253,.T.);
#2395=EDGE_CURVE('',#1906,#1903,#254,.T.);
#2396=EDGE_CURVE('',#1884,#1925,#255,.T.);
#2397=EDGE_CURVE('',#1901,#1899,#256,.T.);
#2398=EDGE_CURVE('',#1902,#1907,#257,.T.);
#2399=EDGE_CURVE('',#1898,#1900,#258,.T.);
#2400=EDGE_CURVE('',#1924,#1885,#259,.T.);
#2401=EDGE_CURVE('',#1926,#1926,#1645,.T.);
#2402=EDGE_CURVE('',#1927,#1927,#1646,.T.);
#2403=EDGE_CURVE('',#1928,#1928,#1647,.T.);
#2404=EDGE_CURVE('',#1929,#1929,#1648,.T.);
#2405=EDGE_CURVE('',#1930,#1930,#1649,.T.);
#2406=EDGE_CURVE('',#1927,#1929,#1198,.T.);
#2407=EDGE_CURVE('',#1930,#1931,#1199,.T.);
#2408=EDGE_CURVE('',#1931,#1931,#1650,.T.);
#2409=EDGE_CURVE('',#1932,#1932,#1651,.T.);
#2410=EDGE_CURVE('',#1933,#1933,#1652,.T.);
#2411=EDGE_CURVE('',#1926,#1932,#1200,.T.);
#2412=EDGE_CURVE('',#1933,#1928,#1201,.T.);
#2413=EDGE_CURVE('',#1934,#1935,#1202,.T.);
#2414=EDGE_CURVE('',#1934,#1936,#260,.T.);
#2415=EDGE_CURVE('',#1936,#1937,#1653,.F.);
#2416=EDGE_CURVE('',#1937,#1935,#261,.T.);
#2417=EDGE_CURVE('',#1938,#1939,#1203,.T.);
#2418=EDGE_CURVE('',#1938,#1934,#262,.T.);
#2419=EDGE_CURVE('',#1935,#1939,#263,.T.);
#2420=EDGE_CURVE('',#1940,#1941,#1204,.T.);
#2421=EDGE_CURVE('',#1940,#1938,#264,.T.);
#2422=EDGE_CURVE('',#1939,#1941,#265,.T.);
#2423=EDGE_CURVE('',#1942,#1943,#1205,.T.);
#2424=EDGE_CURVE('',#1942,#1940,#266,.T.);
#2425=EDGE_CURVE('',#1941,#1943,#267,.T.);
#2426=EDGE_CURVE('',#1944,#1945,#1206,.T.);
#2427=EDGE_CURVE('',#1944,#1942,#268,.T.);
#2428=EDGE_CURVE('',#1943,#1945,#269,.T.);
#2429=EDGE_CURVE('',#1946,#1947,#1207,.T.);
#2430=EDGE_CURVE('',#1946,#1944,#270,.T.);
#2431=EDGE_CURVE('',#1945,#1947,#271,.T.);
#2432=EDGE_CURVE('',#1948,#1949,#1208,.T.);
#2433=EDGE_CURVE('',#1948,#1946,#272,.T.);
#2434=EDGE_CURVE('',#1947,#1949,#273,.T.);
#2435=EDGE_CURVE('',#1950,#1951,#1209,.T.);
#2436=EDGE_CURVE('',#1950,#1948,#274,.T.);
#2437=EDGE_CURVE('',#1949,#1951,#275,.T.);
#2438=EDGE_CURVE('',#1952,#1953,#1210,.T.);
#2439=EDGE_CURVE('',#1952,#1950,#276,.T.);
#2440=EDGE_CURVE('',#1951,#1953,#277,.T.);
#2441=EDGE_CURVE('',#1954,#1955,#1211,.T.);
#2442=EDGE_CURVE('',#1954,#1952,#278,.T.);
#2443=EDGE_CURVE('',#1953,#1955,#279,.T.);
#2444=EDGE_CURVE('',#1956,#1957,#1212,.T.);
#2445=EDGE_CURVE('',#1956,#1954,#280,.T.);
#2446=EDGE_CURVE('',#1955,#1957,#281,.T.);
#2447=EDGE_CURVE('',#1958,#1959,#1213,.T.);
#2448=EDGE_CURVE('',#1958,#1960,#282,.T.);
#2449=EDGE_CURVE('',#1960,#1961,#1654,.T.);
#2450=EDGE_CURVE('',#1959,#1961,#283,.T.);
#2451=EDGE_CURVE('',#1962,#1963,#1214,.T.);
#2452=EDGE_CURVE('',#1962,#1958,#284,.T.);
#2453=EDGE_CURVE('',#1963,#1959,#285,.T.);
#2454=EDGE_CURVE('',#1964,#1965,#1215,.T.);
#2455=EDGE_CURVE('',#1964,#1962,#286,.T.);
#2456=EDGE_CURVE('',#1965,#1963,#287,.T.);
#2457=EDGE_CURVE('',#1966,#1967,#1216,.T.);
#2458=EDGE_CURVE('',#1966,#1964,#288,.T.);
#2459=EDGE_CURVE('',#1967,#1965,#289,.T.);
#2460=EDGE_CURVE('',#1968,#1969,#1217,.T.);
#2461=EDGE_CURVE('',#1968,#1966,#290,.T.);
#2462=EDGE_CURVE('',#1969,#1967,#291,.T.);
#2463=EDGE_CURVE('',#1970,#1971,#1218,.T.);
#2464=EDGE_CURVE('',#1970,#1968,#292,.T.);
#2465=EDGE_CURVE('',#1971,#1969,#293,.T.);
#2466=EDGE_CURVE('',#1972,#1973,#1219,.T.);
#2467=EDGE_CURVE('',#1972,#1970,#294,.T.);
#2468=EDGE_CURVE('',#1973,#1971,#295,.T.);
#2469=EDGE_CURVE('',#1974,#1975,#1220,.T.);
#2470=EDGE_CURVE('',#1974,#1972,#296,.T.);
#2471=EDGE_CURVE('',#1975,#1973,#297,.T.);
#2472=EDGE_CURVE('',#1976,#1977,#1221,.T.);
#2473=EDGE_CURVE('',#1976,#1974,#298,.T.);
#2474=EDGE_CURVE('',#1977,#1975,#299,.T.);
#2475=EDGE_CURVE('',#1978,#1979,#1222,.T.);
#2476=EDGE_CURVE('',#1978,#1976,#300,.T.);
#2477=EDGE_CURVE('',#1979,#1977,#301,.T.);
#2478=EDGE_CURVE('',#1980,#1981,#1223,.T.);
#2479=EDGE_CURVE('',#1980,#1978,#302,.T.);
#2480=EDGE_CURVE('',#1981,#1979,#303,.T.);
#2481=EDGE_CURVE('',#1961,#1982,#304,.T.);
#2482=EDGE_CURVE('',#1983,#1960,#305,.T.);
#2483=EDGE_CURVE('',#1984,#1983,#1655,.T.);
#2484=EDGE_CURVE('',#1982,#1984,#306,.T.);
#2485=EDGE_CURVE('',#1982,#1985,#1224,.T.);
#2486=EDGE_CURVE('',#1985,#1985,#1656,.T.);
#2487=EDGE_CURVE('',#1986,#1980,#307,.T.);
#2488=EDGE_CURVE('',#1936,#1986,#308,.T.);
#2489=EDGE_CURVE('',#1983,#1956,#309,.T.);
#2490=EDGE_CURVE('',#1987,#1981,#310,.T.);
#2491=EDGE_CURVE('',#1986,#1987,#1657,.T.);
#2492=EDGE_CURVE('',#1957,#1984,#311,.T.);
#2493=EDGE_CURVE('',#1987,#1937,#312,.T.);
#2494=EDGE_CURVE('',#1988,#1989,#1225,.T.);
#2495=EDGE_CURVE('',#1988,#1990,#1226,.T.);
#2496=EDGE_CURVE('',#1990,#1991,#1227,.T.);
#2497=EDGE_CURVE('',#1989,#1991,#1228,.T.);
#2498=EDGE_CURVE('',#1992,#1988,#1229,.T.);
#2499=EDGE_CURVE('',#1992,#1993,#1230,.T.);
#2500=EDGE_CURVE('',#1993,#1990,#1231,.T.);
#2501=EDGE_CURVE('',#1994,#1992,#1232,.T.);
#2502=EDGE_CURVE('',#1994,#1995,#1233,.T.);
#2503=EDGE_CURVE('',#1995,#1993,#1234,.T.);
#2504=EDGE_CURVE('',#1996,#1994,#1235,.T.);
#2505=EDGE_CURVE('',#1996,#1997,#1236,.T.);
#2506=EDGE_CURVE('',#1997,#1995,#1237,.T.);
#2507=EDGE_CURVE('',#1998,#1996,#1238,.T.);
#2508=EDGE_CURVE('',#1998,#1999,#1239,.T.);
#2509=EDGE_CURVE('',#1999,#1997,#1240,.T.);
#2510=EDGE_CURVE('',#1989,#1998,#1241,.T.);
#2511=EDGE_CURVE('',#1991,#1999,#1242,.T.);
#2512=EDGE_CURVE('',#2000,#2000,#1658,.T.);
#2513=EDGE_CURVE('',#2000,#2001,#1243,.T.);
#2514=EDGE_CURVE('',#2001,#2001,#1659,.T.);
#2515=ORIENTED_EDGE('',*,*,#2002,.T.);
#2516=ORIENTED_EDGE('',*,*,#2003,.T.);
#2517=ORIENTED_EDGE('',*,*,#2004,.T.);
#2518=ORIENTED_EDGE('',*,*,#2005,.T.);
#2519=ORIENTED_EDGE('',*,*,#2003,.F.);
#2520=ORIENTED_EDGE('',*,*,#2006,.F.);
#2521=ORIENTED_EDGE('',*,*,#2007,.F.);
#2522=ORIENTED_EDGE('',*,*,#2008,.T.);
#2523=ORIENTED_EDGE('',*,*,#2002,.F.);
#2524=ORIENTED_EDGE('',*,*,#2009,.T.);
#2525=ORIENTED_EDGE('',*,*,#2010,.F.);
#2526=ORIENTED_EDGE('',*,*,#2011,.T.);
#2527=ORIENTED_EDGE('',*,*,#2012,.F.);
#2528=ORIENTED_EDGE('',*,*,#2013,.T.);
#2529=ORIENTED_EDGE('',*,*,#2014,.F.);
#2530=ORIENTED_EDGE('',*,*,#2006,.T.);
#2531=ORIENTED_EDGE('',*,*,#2015,.T.);
#2532=ORIENTED_EDGE('',*,*,#2016,.F.);
#2533=ORIENTED_EDGE('',*,*,#2017,.T.);
#2534=ORIENTED_EDGE('',*,*,#2018,.F.);
#2535=ORIENTED_EDGE('',*,*,#2019,.T.);
#2536=ORIENTED_EDGE('',*,*,#2020,.F.);
#2537=ORIENTED_EDGE('',*,*,#2021,.T.);
#2538=ORIENTED_EDGE('',*,*,#2022,.F.);
#2539=ORIENTED_EDGE('',*,*,#2010,.T.);
#2540=ORIENTED_EDGE('',*,*,#2023,.T.);
#2541=ORIENTED_EDGE('',*,*,#2024,.T.);
#2542=ORIENTED_EDGE('',*,*,#2025,.T.);
#2543=ORIENTED_EDGE('',*,*,#2025,.F.);
#2544=ORIENTED_EDGE('',*,*,#2026,.T.);
#2545=ORIENTED_EDGE('',*,*,#2027,.F.);
#2546=ORIENTED_EDGE('',*,*,#2011,.F.);
#2547=ORIENTED_EDGE('',*,*,#2012,.T.);
#2548=ORIENTED_EDGE('',*,*,#2027,.T.);
#2549=ORIENTED_EDGE('',*,*,#2028,.T.);
#2550=ORIENTED_EDGE('',*,*,#2029,.T.);
#2551=ORIENTED_EDGE('',*,*,#2014,.T.);
#2552=ORIENTED_EDGE('',*,*,#2030,.T.);
#2553=ORIENTED_EDGE('',*,*,#2031,.T.);
#2554=ORIENTED_EDGE('',*,*,#2007,.T.);
#2555=ORIENTED_EDGE('',*,*,#2032,.T.);
#2556=ORIENTED_EDGE('',*,*,#2033,.T.);
#2557=ORIENTED_EDGE('',*,*,#2016,.T.);
#2558=ORIENTED_EDGE('',*,*,#2034,.T.);
#2559=ORIENTED_EDGE('',*,*,#2033,.F.);
#2560=ORIENTED_EDGE('',*,*,#2035,.T.);
#2561=ORIENTED_EDGE('',*,*,#2036,.F.);
#2562=ORIENTED_EDGE('',*,*,#2017,.F.);
#2563=ORIENTED_EDGE('',*,*,#2037,.T.);
#2564=ORIENTED_EDGE('',*,*,#2038,.T.);
#2565=ORIENTED_EDGE('',*,*,#2018,.T.);
#2566=ORIENTED_EDGE('',*,*,#2036,.T.);
#2567=ORIENTED_EDGE('',*,*,#2038,.F.);
#2568=ORIENTED_EDGE('',*,*,#2039,.T.);
#2569=ORIENTED_EDGE('',*,*,#2040,.F.);
#2570=ORIENTED_EDGE('',*,*,#2019,.F.);
#2571=ORIENTED_EDGE('',*,*,#2041,.T.);
#2572=ORIENTED_EDGE('',*,*,#2042,.T.);
#2573=ORIENTED_EDGE('',*,*,#2020,.T.);
#2574=ORIENTED_EDGE('',*,*,#2040,.T.);
#2575=ORIENTED_EDGE('',*,*,#2042,.F.);
#2576=ORIENTED_EDGE('',*,*,#2043,.T.);
#2577=ORIENTED_EDGE('',*,*,#2044,.F.);
#2578=ORIENTED_EDGE('',*,*,#2021,.F.);
#2579=ORIENTED_EDGE('',*,*,#2045,.T.);
#2580=ORIENTED_EDGE('',*,*,#2046,.T.);
#2581=ORIENTED_EDGE('',*,*,#2022,.T.);
#2582=ORIENTED_EDGE('',*,*,#2044,.T.);
#2583=ORIENTED_EDGE('',*,*,#2034,.F.);
#2584=ORIENTED_EDGE('',*,*,#2015,.F.);
#2585=ORIENTED_EDGE('',*,*,#2046,.F.);
#2586=ORIENTED_EDGE('',*,*,#2047,.T.);
#2587=ORIENTED_EDGE('',*,*,#2029,.F.);
#2588=ORIENTED_EDGE('',*,*,#2048,.T.);
#2589=ORIENTED_EDGE('',*,*,#2030,.F.);
#2590=ORIENTED_EDGE('',*,*,#2013,.F.);
#2591=ORIENTED_EDGE('',*,*,#2005,.F.);
#2592=ORIENTED_EDGE('',*,*,#2049,.T.);
#2593=ORIENTED_EDGE('',*,*,#2023,.F.);
#2594=ORIENTED_EDGE('',*,*,#2009,.F.);
#2595=ORIENTED_EDGE('',*,*,#2004,.F.);
#2596=ORIENTED_EDGE('',*,*,#2008,.F.);
#2597=ORIENTED_EDGE('',*,*,#2031,.F.);
#2598=ORIENTED_EDGE('',*,*,#2048,.F.);
#2599=ORIENTED_EDGE('',*,*,#2028,.F.);
#2600=ORIENTED_EDGE('',*,*,#2026,.F.);
#2601=ORIENTED_EDGE('',*,*,#2024,.F.);
#2602=ORIENTED_EDGE('',*,*,#2049,.F.);
#2603=ORIENTED_EDGE('',*,*,#2045,.F.);
#2604=ORIENTED_EDGE('',*,*,#2043,.F.);
#2605=ORIENTED_EDGE('',*,*,#2041,.F.);
#2606=ORIENTED_EDGE('',*,*,#2039,.F.);
#2607=ORIENTED_EDGE('',*,*,#2037,.F.);
#2608=ORIENTED_EDGE('',*,*,#2035,.F.);
#2609=ORIENTED_EDGE('',*,*,#2032,.F.);
#2610=ORIENTED_EDGE('',*,*,#2047,.F.);
#2611=ORIENTED_EDGE('',*,*,#2050,.F.);
#2612=ORIENTED_EDGE('',*,*,#2051,.T.);
#2613=ORIENTED_EDGE('',*,*,#2052,.F.);
#2614=ORIENTED_EDGE('',*,*,#2051,.F.);
#2615=ORIENTED_EDGE('',*,*,#2053,.F.);
#2616=ORIENTED_EDGE('',*,*,#2054,.T.);
#2617=ORIENTED_EDGE('',*,*,#2055,.F.);
#2618=ORIENTED_EDGE('',*,*,#2054,.F.);
#2619=ORIENTED_EDGE('',*,*,#2056,.T.);
#2620=ORIENTED_EDGE('',*,*,#2057,.T.);
#2621=ORIENTED_EDGE('',*,*,#2058,.T.);
#2622=ORIENTED_EDGE('',*,*,#2059,.T.);
#2623=ORIENTED_EDGE('',*,*,#2057,.F.);
#2624=ORIENTED_EDGE('',*,*,#2060,.F.);
#2625=ORIENTED_EDGE('',*,*,#2061,.F.);
#2626=ORIENTED_EDGE('',*,*,#2062,.T.);
#2627=ORIENTED_EDGE('',*,*,#2056,.F.);
#2628=ORIENTED_EDGE('',*,*,#2063,.T.);
#2629=ORIENTED_EDGE('',*,*,#2064,.F.);
#2630=ORIENTED_EDGE('',*,*,#2065,.T.);
#2631=ORIENTED_EDGE('',*,*,#2066,.F.);
#2632=ORIENTED_EDGE('',*,*,#2067,.T.);
#2633=ORIENTED_EDGE('',*,*,#2068,.F.);
#2634=ORIENTED_EDGE('',*,*,#2060,.T.);
#2635=ORIENTED_EDGE('',*,*,#2069,.T.);
#2636=ORIENTED_EDGE('',*,*,#2070,.F.);
#2637=ORIENTED_EDGE('',*,*,#2071,.T.);
#2638=ORIENTED_EDGE('',*,*,#2072,.F.);
#2639=ORIENTED_EDGE('',*,*,#2073,.T.);
#2640=ORIENTED_EDGE('',*,*,#2074,.F.);
#2641=ORIENTED_EDGE('',*,*,#2075,.T.);
#2642=ORIENTED_EDGE('',*,*,#2076,.F.);
#2643=ORIENTED_EDGE('',*,*,#2064,.T.);
#2644=ORIENTED_EDGE('',*,*,#2077,.T.);
#2645=ORIENTED_EDGE('',*,*,#2078,.T.);
#2646=ORIENTED_EDGE('',*,*,#2079,.T.);
#2647=ORIENTED_EDGE('',*,*,#2079,.F.);
#2648=ORIENTED_EDGE('',*,*,#2080,.T.);
#2649=ORIENTED_EDGE('',*,*,#2081,.F.);
#2650=ORIENTED_EDGE('',*,*,#2065,.F.);
#2651=ORIENTED_EDGE('',*,*,#2066,.T.);
#2652=ORIENTED_EDGE('',*,*,#2081,.T.);
#2653=ORIENTED_EDGE('',*,*,#2082,.T.);
#2654=ORIENTED_EDGE('',*,*,#2083,.T.);
#2655=ORIENTED_EDGE('',*,*,#2068,.T.);
#2656=ORIENTED_EDGE('',*,*,#2084,.T.);
#2657=ORIENTED_EDGE('',*,*,#2085,.T.);
#2658=ORIENTED_EDGE('',*,*,#2061,.T.);
#2659=ORIENTED_EDGE('',*,*,#2086,.T.);
#2660=ORIENTED_EDGE('',*,*,#2087,.T.);
#2661=ORIENTED_EDGE('',*,*,#2070,.T.);
#2662=ORIENTED_EDGE('',*,*,#2088,.T.);
#2663=ORIENTED_EDGE('',*,*,#2087,.F.);
#2664=ORIENTED_EDGE('',*,*,#2089,.T.);
#2665=ORIENTED_EDGE('',*,*,#2090,.F.);
#2666=ORIENTED_EDGE('',*,*,#2071,.F.);
#2667=ORIENTED_EDGE('',*,*,#2052,.T.);
#2668=ORIENTED_EDGE('',*,*,#2055,.T.);
#2669=ORIENTED_EDGE('',*,*,#2091,.T.);
#2670=ORIENTED_EDGE('',*,*,#2092,.T.);
#2671=ORIENTED_EDGE('',*,*,#2072,.T.);
#2672=ORIENTED_EDGE('',*,*,#2090,.T.);
#2673=ORIENTED_EDGE('',*,*,#2092,.F.);
#2674=ORIENTED_EDGE('',*,*,#2093,.T.);
#2675=ORIENTED_EDGE('',*,*,#2094,.F.);
#2676=ORIENTED_EDGE('',*,*,#2073,.F.);
#2677=ORIENTED_EDGE('',*,*,#2095,.T.);
#2678=ORIENTED_EDGE('',*,*,#2096,.T.);
#2679=ORIENTED_EDGE('',*,*,#2074,.T.);
#2680=ORIENTED_EDGE('',*,*,#2094,.T.);
#2681=ORIENTED_EDGE('',*,*,#2096,.F.);
#2682=ORIENTED_EDGE('',*,*,#2097,.T.);
#2683=ORIENTED_EDGE('',*,*,#2098,.F.);
#2684=ORIENTED_EDGE('',*,*,#2075,.F.);
#2685=ORIENTED_EDGE('',*,*,#2099,.T.);
#2686=ORIENTED_EDGE('',*,*,#2100,.T.);
#2687=ORIENTED_EDGE('',*,*,#2076,.T.);
#2688=ORIENTED_EDGE('',*,*,#2098,.T.);
#2689=ORIENTED_EDGE('',*,*,#2088,.F.);
#2690=ORIENTED_EDGE('',*,*,#2069,.F.);
#2691=ORIENTED_EDGE('',*,*,#2100,.F.);
#2692=ORIENTED_EDGE('',*,*,#2101,.T.);
#2693=ORIENTED_EDGE('',*,*,#2083,.F.);
#2694=ORIENTED_EDGE('',*,*,#2102,.T.);
#2695=ORIENTED_EDGE('',*,*,#2084,.F.);
#2696=ORIENTED_EDGE('',*,*,#2067,.F.);
#2697=ORIENTED_EDGE('',*,*,#2050,.T.);
#2698=ORIENTED_EDGE('',*,*,#2053,.T.);
#2699=ORIENTED_EDGE('',*,*,#2059,.F.);
#2700=ORIENTED_EDGE('',*,*,#2103,.T.);
#2701=ORIENTED_EDGE('',*,*,#2077,.F.);
#2702=ORIENTED_EDGE('',*,*,#2063,.F.);
#2703=ORIENTED_EDGE('',*,*,#2058,.F.);
#2704=ORIENTED_EDGE('',*,*,#2062,.F.);
#2705=ORIENTED_EDGE('',*,*,#2085,.F.);
#2706=ORIENTED_EDGE('',*,*,#2102,.F.);
#2707=ORIENTED_EDGE('',*,*,#2082,.F.);
#2708=ORIENTED_EDGE('',*,*,#2080,.F.);
#2709=ORIENTED_EDGE('',*,*,#2078,.F.);
#2710=ORIENTED_EDGE('',*,*,#2103,.F.);
#2711=ORIENTED_EDGE('',*,*,#2099,.F.);
#2712=ORIENTED_EDGE('',*,*,#2097,.F.);
#2713=ORIENTED_EDGE('',*,*,#2095,.F.);
#2714=ORIENTED_EDGE('',*,*,#2093,.F.);
#2715=ORIENTED_EDGE('',*,*,#2091,.F.);
#2716=ORIENTED_EDGE('',*,*,#2089,.F.);
#2717=ORIENTED_EDGE('',*,*,#2086,.F.);
#2718=ORIENTED_EDGE('',*,*,#2101,.F.);
#2719=ORIENTED_EDGE('',*,*,#2104,.T.);
#2720=ORIENTED_EDGE('',*,*,#2105,.T.);
#2721=ORIENTED_EDGE('',*,*,#2106,.T.);
#2722=ORIENTED_EDGE('',*,*,#2107,.T.);
#2723=ORIENTED_EDGE('',*,*,#2105,.F.);
#2724=ORIENTED_EDGE('',*,*,#2108,.F.);
#2725=ORIENTED_EDGE('',*,*,#2109,.F.);
#2726=ORIENTED_EDGE('',*,*,#2110,.T.);
#2727=ORIENTED_EDGE('',*,*,#2104,.F.);
#2728=ORIENTED_EDGE('',*,*,#2111,.T.);
#2729=ORIENTED_EDGE('',*,*,#2112,.F.);
#2730=ORIENTED_EDGE('',*,*,#2113,.T.);
#2731=ORIENTED_EDGE('',*,*,#2114,.F.);
#2732=ORIENTED_EDGE('',*,*,#2115,.T.);
#2733=ORIENTED_EDGE('',*,*,#2116,.F.);
#2734=ORIENTED_EDGE('',*,*,#2108,.T.);
#2735=ORIENTED_EDGE('',*,*,#2117,.T.);
#2736=ORIENTED_EDGE('',*,*,#2118,.F.);
#2737=ORIENTED_EDGE('',*,*,#2119,.T.);
#2738=ORIENTED_EDGE('',*,*,#2120,.F.);
#2739=ORIENTED_EDGE('',*,*,#2121,.T.);
#2740=ORIENTED_EDGE('',*,*,#2122,.F.);
#2741=ORIENTED_EDGE('',*,*,#2123,.T.);
#2742=ORIENTED_EDGE('',*,*,#2124,.F.);
#2743=ORIENTED_EDGE('',*,*,#2112,.T.);
#2744=ORIENTED_EDGE('',*,*,#2125,.T.);
#2745=ORIENTED_EDGE('',*,*,#2126,.T.);
#2746=ORIENTED_EDGE('',*,*,#2127,.T.);
#2747=ORIENTED_EDGE('',*,*,#2127,.F.);
#2748=ORIENTED_EDGE('',*,*,#2128,.T.);
#2749=ORIENTED_EDGE('',*,*,#2129,.F.);
#2750=ORIENTED_EDGE('',*,*,#2113,.F.);
#2751=ORIENTED_EDGE('',*,*,#2114,.T.);
#2752=ORIENTED_EDGE('',*,*,#2129,.T.);
#2753=ORIENTED_EDGE('',*,*,#2130,.T.);
#2754=ORIENTED_EDGE('',*,*,#2131,.T.);
#2755=ORIENTED_EDGE('',*,*,#2116,.T.);
#2756=ORIENTED_EDGE('',*,*,#2132,.T.);
#2757=ORIENTED_EDGE('',*,*,#2133,.T.);
#2758=ORIENTED_EDGE('',*,*,#2109,.T.);
#2759=ORIENTED_EDGE('',*,*,#2134,.T.);
#2760=ORIENTED_EDGE('',*,*,#2135,.T.);
#2761=ORIENTED_EDGE('',*,*,#2118,.T.);
#2762=ORIENTED_EDGE('',*,*,#2136,.T.);
#2763=ORIENTED_EDGE('',*,*,#2135,.F.);
#2764=ORIENTED_EDGE('',*,*,#2137,.T.);
#2765=ORIENTED_EDGE('',*,*,#2138,.F.);
#2766=ORIENTED_EDGE('',*,*,#2119,.F.);
#2767=ORIENTED_EDGE('',*,*,#2139,.T.);
#2768=ORIENTED_EDGE('',*,*,#2140,.T.);
#2769=ORIENTED_EDGE('',*,*,#2120,.T.);
#2770=ORIENTED_EDGE('',*,*,#2138,.T.);
#2771=ORIENTED_EDGE('',*,*,#2140,.F.);
#2772=ORIENTED_EDGE('',*,*,#2141,.T.);
#2773=ORIENTED_EDGE('',*,*,#2142,.F.);
#2774=ORIENTED_EDGE('',*,*,#2121,.F.);
#2775=ORIENTED_EDGE('',*,*,#2143,.T.);
#2776=ORIENTED_EDGE('',*,*,#2144,.T.);
#2777=ORIENTED_EDGE('',*,*,#2122,.T.);
#2778=ORIENTED_EDGE('',*,*,#2142,.T.);
#2779=ORIENTED_EDGE('',*,*,#2144,.F.);
#2780=ORIENTED_EDGE('',*,*,#2145,.T.);
#2781=ORIENTED_EDGE('',*,*,#2146,.F.);
#2782=ORIENTED_EDGE('',*,*,#2123,.F.);
#2783=ORIENTED_EDGE('',*,*,#2147,.T.);
#2784=ORIENTED_EDGE('',*,*,#2148,.T.);
#2785=ORIENTED_EDGE('',*,*,#2124,.T.);
#2786=ORIENTED_EDGE('',*,*,#2146,.T.);
#2787=ORIENTED_EDGE('',*,*,#2136,.F.);
#2788=ORIENTED_EDGE('',*,*,#2117,.F.);
#2789=ORIENTED_EDGE('',*,*,#2148,.F.);
#2790=ORIENTED_EDGE('',*,*,#2149,.T.);
#2791=ORIENTED_EDGE('',*,*,#2131,.F.);
#2792=ORIENTED_EDGE('',*,*,#2150,.T.);
#2793=ORIENTED_EDGE('',*,*,#2132,.F.);
#2794=ORIENTED_EDGE('',*,*,#2115,.F.);
#2795=ORIENTED_EDGE('',*,*,#2107,.F.);
#2796=ORIENTED_EDGE('',*,*,#2151,.T.);
#2797=ORIENTED_EDGE('',*,*,#2125,.F.);
#2798=ORIENTED_EDGE('',*,*,#2111,.F.);
#2799=ORIENTED_EDGE('',*,*,#2106,.F.);
#2800=ORIENTED_EDGE('',*,*,#2110,.F.);
#2801=ORIENTED_EDGE('',*,*,#2133,.F.);
#2802=ORIENTED_EDGE('',*,*,#2150,.F.);
#2803=ORIENTED_EDGE('',*,*,#2130,.F.);
#2804=ORIENTED_EDGE('',*,*,#2128,.F.);
#2805=ORIENTED_EDGE('',*,*,#2126,.F.);
#2806=ORIENTED_EDGE('',*,*,#2151,.F.);
#2807=ORIENTED_EDGE('',*,*,#2147,.F.);
#2808=ORIENTED_EDGE('',*,*,#2145,.F.);
#2809=ORIENTED_EDGE('',*,*,#2143,.F.);
#2810=ORIENTED_EDGE('',*,*,#2141,.F.);
#2811=ORIENTED_EDGE('',*,*,#2139,.F.);
#2812=ORIENTED_EDGE('',*,*,#2137,.F.);
#2813=ORIENTED_EDGE('',*,*,#2134,.F.);
#2814=ORIENTED_EDGE('',*,*,#2149,.F.);
#2815=ORIENTED_EDGE('',*,*,#2152,.F.);
#2816=ORIENTED_EDGE('',*,*,#2153,.T.);
#2817=ORIENTED_EDGE('',*,*,#2154,.F.);
#2818=ORIENTED_EDGE('',*,*,#2153,.F.);
#2819=ORIENTED_EDGE('',*,*,#2155,.F.);
#2820=ORIENTED_EDGE('',*,*,#2156,.T.);
#2821=ORIENTED_EDGE('',*,*,#2157,.F.);
#2822=ORIENTED_EDGE('',*,*,#2156,.F.);
#2823=ORIENTED_EDGE('',*,*,#2158,.T.);
#2824=ORIENTED_EDGE('',*,*,#2159,.T.);
#2825=ORIENTED_EDGE('',*,*,#2160,.T.);
#2826=ORIENTED_EDGE('',*,*,#2161,.T.);
#2827=ORIENTED_EDGE('',*,*,#2158,.F.);
#2828=ORIENTED_EDGE('',*,*,#2162,.T.);
#2829=ORIENTED_EDGE('',*,*,#2163,.F.);
#2830=ORIENTED_EDGE('',*,*,#2164,.T.);
#2831=ORIENTED_EDGE('',*,*,#2165,.F.);
#2832=ORIENTED_EDGE('',*,*,#2166,.T.);
#2833=ORIENTED_EDGE('',*,*,#2167,.F.);
#2834=ORIENTED_EDGE('',*,*,#2168,.T.);
#2835=ORIENTED_EDGE('',*,*,#2169,.F.);
#2836=ORIENTED_EDGE('',*,*,#2170,.T.);
#2837=ORIENTED_EDGE('',*,*,#2171,.F.);
#2838=ORIENTED_EDGE('',*,*,#2172,.T.);
#2839=ORIENTED_EDGE('',*,*,#2173,.F.);
#2840=ORIENTED_EDGE('',*,*,#2174,.T.);
#2841=ORIENTED_EDGE('',*,*,#2175,.F.);
#2842=ORIENTED_EDGE('',*,*,#2176,.T.);
#2843=ORIENTED_EDGE('',*,*,#2161,.F.);
#2844=ORIENTED_EDGE('',*,*,#2177,.T.);
#2845=ORIENTED_EDGE('',*,*,#2178,.F.);
#2846=ORIENTED_EDGE('',*,*,#2162,.F.);
#2847=ORIENTED_EDGE('',*,*,#2154,.T.);
#2848=ORIENTED_EDGE('',*,*,#2157,.T.);
#2849=ORIENTED_EDGE('',*,*,#2163,.T.);
#2850=ORIENTED_EDGE('',*,*,#2178,.T.);
#2851=ORIENTED_EDGE('',*,*,#2179,.T.);
#2852=ORIENTED_EDGE('',*,*,#2180,.T.);
#2853=ORIENTED_EDGE('',*,*,#2165,.T.);
#2854=ORIENTED_EDGE('',*,*,#2181,.T.);
#2855=ORIENTED_EDGE('',*,*,#2182,.T.);
#2856=ORIENTED_EDGE('',*,*,#2183,.T.);
#2857=ORIENTED_EDGE('',*,*,#2183,.F.);
#2858=ORIENTED_EDGE('',*,*,#2184,.T.);
#2859=ORIENTED_EDGE('',*,*,#2185,.F.);
#2860=ORIENTED_EDGE('',*,*,#2166,.F.);
#2861=ORIENTED_EDGE('',*,*,#2167,.T.);
#2862=ORIENTED_EDGE('',*,*,#2185,.T.);
#2863=ORIENTED_EDGE('',*,*,#2186,.T.);
#2864=ORIENTED_EDGE('',*,*,#2187,.T.);
#2865=ORIENTED_EDGE('',*,*,#2188,.T.);
#2866=ORIENTED_EDGE('',*,*,#2189,.T.);
#2867=ORIENTED_EDGE('',*,*,#2169,.T.);
#2868=ORIENTED_EDGE('',*,*,#2190,.T.);
#2869=ORIENTED_EDGE('',*,*,#2189,.F.);
#2870=ORIENTED_EDGE('',*,*,#2191,.T.);
#2871=ORIENTED_EDGE('',*,*,#2192,.F.);
#2872=ORIENTED_EDGE('',*,*,#2170,.F.);
#2873=ORIENTED_EDGE('',*,*,#2152,.T.);
#2874=ORIENTED_EDGE('',*,*,#2155,.T.);
#2875=ORIENTED_EDGE('',*,*,#2193,.T.);
#2876=ORIENTED_EDGE('',*,*,#2194,.T.);
#2877=ORIENTED_EDGE('',*,*,#2171,.T.);
#2878=ORIENTED_EDGE('',*,*,#2192,.T.);
#2879=ORIENTED_EDGE('',*,*,#2194,.F.);
#2880=ORIENTED_EDGE('',*,*,#2195,.T.);
#2881=ORIENTED_EDGE('',*,*,#2196,.F.);
#2882=ORIENTED_EDGE('',*,*,#2172,.F.);
#2883=ORIENTED_EDGE('',*,*,#2173,.T.);
#2884=ORIENTED_EDGE('',*,*,#2196,.T.);
#2885=ORIENTED_EDGE('',*,*,#2197,.T.);
#2886=ORIENTED_EDGE('',*,*,#2198,.T.);
#2887=ORIENTED_EDGE('',*,*,#2175,.T.);
#2888=ORIENTED_EDGE('',*,*,#2199,.T.);
#2889=ORIENTED_EDGE('',*,*,#2200,.T.);
#2890=ORIENTED_EDGE('',*,*,#2201,.T.);
#2891=ORIENTED_EDGE('',*,*,#2159,.F.);
#2892=ORIENTED_EDGE('',*,*,#2176,.F.);
#2893=ORIENTED_EDGE('',*,*,#2201,.F.);
#2894=ORIENTED_EDGE('',*,*,#2202,.T.);
#2895=ORIENTED_EDGE('',*,*,#2198,.F.);
#2896=ORIENTED_EDGE('',*,*,#2203,.T.);
#2897=ORIENTED_EDGE('',*,*,#2199,.F.);
#2898=ORIENTED_EDGE('',*,*,#2174,.F.);
#2899=ORIENTED_EDGE('',*,*,#2187,.F.);
#2900=ORIENTED_EDGE('',*,*,#2204,.T.);
#2901=ORIENTED_EDGE('',*,*,#2190,.F.);
#2902=ORIENTED_EDGE('',*,*,#2168,.F.);
#2903=ORIENTED_EDGE('',*,*,#2180,.F.);
#2904=ORIENTED_EDGE('',*,*,#2205,.T.);
#2905=ORIENTED_EDGE('',*,*,#2181,.F.);
#2906=ORIENTED_EDGE('',*,*,#2164,.F.);
#2907=ORIENTED_EDGE('',*,*,#2160,.F.);
#2908=ORIENTED_EDGE('',*,*,#2202,.F.);
#2909=ORIENTED_EDGE('',*,*,#2200,.F.);
#2910=ORIENTED_EDGE('',*,*,#2203,.F.);
#2911=ORIENTED_EDGE('',*,*,#2197,.F.);
#2912=ORIENTED_EDGE('',*,*,#2195,.F.);
#2913=ORIENTED_EDGE('',*,*,#2193,.F.);
#2914=ORIENTED_EDGE('',*,*,#2191,.F.);
#2915=ORIENTED_EDGE('',*,*,#2188,.F.);
#2916=ORIENTED_EDGE('',*,*,#2204,.F.);
#2917=ORIENTED_EDGE('',*,*,#2186,.F.);
#2918=ORIENTED_EDGE('',*,*,#2184,.F.);
#2919=ORIENTED_EDGE('',*,*,#2182,.F.);
#2920=ORIENTED_EDGE('',*,*,#2205,.F.);
#2921=ORIENTED_EDGE('',*,*,#2179,.F.);
#2922=ORIENTED_EDGE('',*,*,#2177,.F.);
#2923=ORIENTED_EDGE('',*,*,#2206,.F.);
#2924=ORIENTED_EDGE('',*,*,#2207,.T.);
#2925=ORIENTED_EDGE('',*,*,#2208,.F.);
#2926=ORIENTED_EDGE('',*,*,#2207,.F.);
#2927=ORIENTED_EDGE('',*,*,#2209,.F.);
#2928=ORIENTED_EDGE('',*,*,#2210,.T.);
#2929=ORIENTED_EDGE('',*,*,#2211,.F.);
#2930=ORIENTED_EDGE('',*,*,#2210,.F.);
#2931=ORIENTED_EDGE('',*,*,#2212,.F.);
#2932=ORIENTED_EDGE('',*,*,#2213,.T.);
#2933=ORIENTED_EDGE('',*,*,#2214,.F.);
#2934=ORIENTED_EDGE('',*,*,#2213,.F.);
#2935=ORIENTED_EDGE('',*,*,#2215,.F.);
#2936=ORIENTED_EDGE('',*,*,#2216,.T.);
#2937=ORIENTED_EDGE('',*,*,#2217,.F.);
#2938=ORIENTED_EDGE('',*,*,#2216,.F.);
#2939=ORIENTED_EDGE('',*,*,#2218,.F.);
#2940=ORIENTED_EDGE('',*,*,#2219,.T.);
#2941=ORIENTED_EDGE('',*,*,#2220,.F.);
#2942=ORIENTED_EDGE('',*,*,#2219,.F.);
#2943=ORIENTED_EDGE('',*,*,#2221,.F.);
#2944=ORIENTED_EDGE('',*,*,#2222,.T.);
#2945=ORIENTED_EDGE('',*,*,#2223,.F.);
#2946=ORIENTED_EDGE('',*,*,#2222,.F.);
#2947=ORIENTED_EDGE('',*,*,#2224,.F.);
#2948=ORIENTED_EDGE('',*,*,#2225,.T.);
#2949=ORIENTED_EDGE('',*,*,#2226,.F.);
#2950=ORIENTED_EDGE('',*,*,#2225,.F.);
#2951=ORIENTED_EDGE('',*,*,#2227,.F.);
#2952=ORIENTED_EDGE('',*,*,#2228,.T.);
#2953=ORIENTED_EDGE('',*,*,#2229,.F.);
#2954=ORIENTED_EDGE('',*,*,#2228,.F.);
#2955=ORIENTED_EDGE('',*,*,#2230,.F.);
#2956=ORIENTED_EDGE('',*,*,#2231,.T.);
#2957=ORIENTED_EDGE('',*,*,#2232,.F.);
#2958=ORIENTED_EDGE('',*,*,#2233,.F.);
#2959=ORIENTED_EDGE('',*,*,#2234,.F.);
#2960=ORIENTED_EDGE('',*,*,#2235,.F.);
#2961=ORIENTED_EDGE('',*,*,#2236,.F.);
#2962=ORIENTED_EDGE('',*,*,#2231,.F.);
#2963=ORIENTED_EDGE('',*,*,#2237,.F.);
#2964=ORIENTED_EDGE('',*,*,#2238,.T.);
#2965=ORIENTED_EDGE('',*,*,#2239,.F.);
#2966=ORIENTED_EDGE('',*,*,#2240,.F.);
#2967=ORIENTED_EDGE('',*,*,#2241,.F.);
#2968=ORIENTED_EDGE('',*,*,#2242,.F.);
#2969=ORIENTED_EDGE('',*,*,#2243,.F.);
#2970=ORIENTED_EDGE('',*,*,#2238,.F.);
#2971=ORIENTED_EDGE('',*,*,#2244,.F.);
#2972=ORIENTED_EDGE('',*,*,#2245,.T.);
#2973=ORIENTED_EDGE('',*,*,#2246,.F.);
#2974=ORIENTED_EDGE('',*,*,#2247,.F.);
#2975=ORIENTED_EDGE('',*,*,#2248,.F.);
#2976=ORIENTED_EDGE('',*,*,#2249,.F.);
#2977=ORIENTED_EDGE('',*,*,#2250,.F.);
#2978=ORIENTED_EDGE('',*,*,#2245,.F.);
#2979=ORIENTED_EDGE('',*,*,#2251,.F.);
#2980=ORIENTED_EDGE('',*,*,#2252,.F.);
#2981=ORIENTED_EDGE('',*,*,#2253,.F.);
#2982=ORIENTED_EDGE('',*,*,#2254,.F.);
#2983=ORIENTED_EDGE('',*,*,#2255,.F.);
#2984=ORIENTED_EDGE('',*,*,#2254,.T.);
#2985=ORIENTED_EDGE('',*,*,#2256,.F.);
#2986=ORIENTED_EDGE('',*,*,#2257,.F.);
#2987=ORIENTED_EDGE('',*,*,#2240,.T.);
#2988=ORIENTED_EDGE('',*,*,#2258,.T.);
#2989=ORIENTED_EDGE('',*,*,#2249,.T.);
#2990=ORIENTED_EDGE('',*,*,#2259,.F.);
#2991=ORIENTED_EDGE('',*,*,#2242,.T.);
#2992=ORIENTED_EDGE('',*,*,#2260,.F.);
#2993=ORIENTED_EDGE('',*,*,#2257,.T.);
#2994=ORIENTED_EDGE('',*,*,#2261,.T.);
#2995=ORIENTED_EDGE('',*,*,#2232,.T.);
#2996=ORIENTED_EDGE('',*,*,#2236,.T.);
#2997=ORIENTED_EDGE('',*,*,#2262,.F.);
#2998=ORIENTED_EDGE('',*,*,#2246,.T.);
#2999=ORIENTED_EDGE('',*,*,#2250,.T.);
#3000=ORIENTED_EDGE('',*,*,#2258,.F.);
#3001=ORIENTED_EDGE('',*,*,#2239,.T.);
#3002=ORIENTED_EDGE('',*,*,#2243,.T.);
#3003=ORIENTED_EDGE('',*,*,#2261,.F.);
#3004=ORIENTED_EDGE('',*,*,#2256,.T.);
#3005=ORIENTED_EDGE('',*,*,#2253,.T.);
#3006=ORIENTED_EDGE('',*,*,#2263,.F.);
#3007=ORIENTED_EDGE('',*,*,#2229,.T.);
#3008=ORIENTED_EDGE('',*,*,#2226,.T.);
#3009=ORIENTED_EDGE('',*,*,#2223,.T.);
#3010=ORIENTED_EDGE('',*,*,#2220,.T.);
#3011=ORIENTED_EDGE('',*,*,#2217,.T.);
#3012=ORIENTED_EDGE('',*,*,#2214,.T.);
#3013=ORIENTED_EDGE('',*,*,#2211,.T.);
#3014=ORIENTED_EDGE('',*,*,#2208,.T.);
#3015=ORIENTED_EDGE('',*,*,#2234,.T.);
#3016=ORIENTED_EDGE('',*,*,#2230,.T.);
#3017=ORIENTED_EDGE('',*,*,#2264,.T.);
#3018=ORIENTED_EDGE('',*,*,#2251,.T.);
#3019=ORIENTED_EDGE('',*,*,#2255,.T.);
#3020=ORIENTED_EDGE('',*,*,#2260,.T.);
#3021=ORIENTED_EDGE('',*,*,#2241,.T.);
#3022=ORIENTED_EDGE('',*,*,#2237,.T.);
#3023=ORIENTED_EDGE('',*,*,#2259,.T.);
#3024=ORIENTED_EDGE('',*,*,#2248,.T.);
#3025=ORIENTED_EDGE('',*,*,#2244,.T.);
#3026=ORIENTED_EDGE('',*,*,#2265,.T.);
#3027=ORIENTED_EDGE('',*,*,#2227,.T.);
#3028=ORIENTED_EDGE('',*,*,#2224,.T.);
#3029=ORIENTED_EDGE('',*,*,#2221,.T.);
#3030=ORIENTED_EDGE('',*,*,#2218,.T.);
#3031=ORIENTED_EDGE('',*,*,#2215,.T.);
#3032=ORIENTED_EDGE('',*,*,#2212,.T.);
#3033=ORIENTED_EDGE('',*,*,#2209,.T.);
#3034=ORIENTED_EDGE('',*,*,#2206,.T.);
#3035=ORIENTED_EDGE('',*,*,#2233,.T.);
#3036=ORIENTED_EDGE('',*,*,#2263,.T.);
#3037=ORIENTED_EDGE('',*,*,#2252,.T.);
#3038=ORIENTED_EDGE('',*,*,#2264,.F.);
#3039=ORIENTED_EDGE('',*,*,#2235,.T.);
#3040=ORIENTED_EDGE('',*,*,#2265,.F.);
#3041=ORIENTED_EDGE('',*,*,#2247,.T.);
#3042=ORIENTED_EDGE('',*,*,#2262,.T.);
#3043=ORIENTED_EDGE('',*,*,#2266,.F.);
#3044=ORIENTED_EDGE('',*,*,#2267,.T.);
#3045=ORIENTED_EDGE('',*,*,#2268,.F.);
#3046=ORIENTED_EDGE('',*,*,#2267,.F.);
#3047=ORIENTED_EDGE('',*,*,#2269,.F.);
#3048=ORIENTED_EDGE('',*,*,#2270,.T.);
#3049=ORIENTED_EDGE('',*,*,#2271,.F.);
#3050=ORIENTED_EDGE('',*,*,#2270,.F.);
#3051=ORIENTED_EDGE('',*,*,#2272,.F.);
#3052=ORIENTED_EDGE('',*,*,#2273,.T.);
#3053=ORIENTED_EDGE('',*,*,#2274,.F.);
#3054=ORIENTED_EDGE('',*,*,#2273,.F.);
#3055=ORIENTED_EDGE('',*,*,#2275,.F.);
#3056=ORIENTED_EDGE('',*,*,#2276,.T.);
#3057=ORIENTED_EDGE('',*,*,#2277,.F.);
#3058=ORIENTED_EDGE('',*,*,#2276,.F.);
#3059=ORIENTED_EDGE('',*,*,#2278,.T.);
#3060=ORIENTED_EDGE('',*,*,#2279,.T.);
#3061=ORIENTED_EDGE('',*,*,#2280,.F.);
#3062=ORIENTED_EDGE('',*,*,#2281,.F.);
#3063=ORIENTED_EDGE('',*,*,#2282,.T.);
#3064=ORIENTED_EDGE('',*,*,#2281,.T.);
#3065=ORIENTED_EDGE('',*,*,#2283,.F.);
#3066=ORIENTED_EDGE('',*,*,#2284,.F.);
#3067=ORIENTED_EDGE('',*,*,#2285,.T.);
#3068=ORIENTED_EDGE('',*,*,#2284,.T.);
#3069=ORIENTED_EDGE('',*,*,#2286,.F.);
#3070=ORIENTED_EDGE('',*,*,#2287,.F.);
#3071=ORIENTED_EDGE('',*,*,#2288,.T.);
#3072=ORIENTED_EDGE('',*,*,#2287,.T.);
#3073=ORIENTED_EDGE('',*,*,#2289,.F.);
#3074=ORIENTED_EDGE('',*,*,#2279,.F.);
#3075=ORIENTED_EDGE('',*,*,#2289,.T.);
#3076=ORIENTED_EDGE('',*,*,#2286,.T.);
#3077=ORIENTED_EDGE('',*,*,#2283,.T.);
#3078=ORIENTED_EDGE('',*,*,#2280,.T.);
#3079=ORIENTED_EDGE('',*,*,#2266,.T.);
#3080=ORIENTED_EDGE('',*,*,#2269,.T.);
#3081=ORIENTED_EDGE('',*,*,#2272,.T.);
#3082=ORIENTED_EDGE('',*,*,#2275,.T.);
#3083=ORIENTED_EDGE('',*,*,#2288,.F.);
#3084=ORIENTED_EDGE('',*,*,#2278,.F.);
#3085=ORIENTED_EDGE('',*,*,#2282,.F.);
#3086=ORIENTED_EDGE('',*,*,#2285,.F.);
#3087=ORIENTED_EDGE('',*,*,#2268,.T.);
#3088=ORIENTED_EDGE('',*,*,#2271,.T.);
#3089=ORIENTED_EDGE('',*,*,#2274,.T.);
#3090=ORIENTED_EDGE('',*,*,#2277,.T.);
#3091=ORIENTED_EDGE('',*,*,#2290,.F.);
#3092=ORIENTED_EDGE('',*,*,#2291,.T.);
#3093=ORIENTED_EDGE('',*,*,#2292,.F.);
#3094=ORIENTED_EDGE('',*,*,#2291,.F.);
#3095=ORIENTED_EDGE('',*,*,#2293,.F.);
#3096=ORIENTED_EDGE('',*,*,#2294,.T.);
#3097=ORIENTED_EDGE('',*,*,#2295,.F.);
#3098=ORIENTED_EDGE('',*,*,#2294,.F.);
#3099=ORIENTED_EDGE('',*,*,#2296,.F.);
#3100=ORIENTED_EDGE('',*,*,#2297,.T.);
#3101=ORIENTED_EDGE('',*,*,#2298,.F.);
#3102=ORIENTED_EDGE('',*,*,#2297,.F.);
#3103=ORIENTED_EDGE('',*,*,#2299,.F.);
#3104=ORIENTED_EDGE('',*,*,#2300,.T.);
#3105=ORIENTED_EDGE('',*,*,#2301,.F.);
#3106=ORIENTED_EDGE('',*,*,#2300,.F.);
#3107=ORIENTED_EDGE('',*,*,#2302,.T.);
#3108=ORIENTED_EDGE('',*,*,#2303,.T.);
#3109=ORIENTED_EDGE('',*,*,#2304,.F.);
#3110=ORIENTED_EDGE('',*,*,#2305,.F.);
#3111=ORIENTED_EDGE('',*,*,#2306,.T.);
#3112=ORIENTED_EDGE('',*,*,#2305,.T.);
#3113=ORIENTED_EDGE('',*,*,#2307,.F.);
#3114=ORIENTED_EDGE('',*,*,#2308,.F.);
#3115=ORIENTED_EDGE('',*,*,#2309,.T.);
#3116=ORIENTED_EDGE('',*,*,#2308,.T.);
#3117=ORIENTED_EDGE('',*,*,#2310,.F.);
#3118=ORIENTED_EDGE('',*,*,#2311,.F.);
#3119=ORIENTED_EDGE('',*,*,#2312,.T.);
#3120=ORIENTED_EDGE('',*,*,#2311,.T.);
#3121=ORIENTED_EDGE('',*,*,#2313,.F.);
#3122=ORIENTED_EDGE('',*,*,#2303,.F.);
#3123=ORIENTED_EDGE('',*,*,#2313,.T.);
#3124=ORIENTED_EDGE('',*,*,#2310,.T.);
#3125=ORIENTED_EDGE('',*,*,#2307,.T.);
#3126=ORIENTED_EDGE('',*,*,#2304,.T.);
#3127=ORIENTED_EDGE('',*,*,#2290,.T.);
#3128=ORIENTED_EDGE('',*,*,#2293,.T.);
#3129=ORIENTED_EDGE('',*,*,#2296,.T.);
#3130=ORIENTED_EDGE('',*,*,#2299,.T.);
#3131=ORIENTED_EDGE('',*,*,#2312,.F.);
#3132=ORIENTED_EDGE('',*,*,#2302,.F.);
#3133=ORIENTED_EDGE('',*,*,#2306,.F.);
#3134=ORIENTED_EDGE('',*,*,#2309,.F.);
#3135=ORIENTED_EDGE('',*,*,#2292,.T.);
#3136=ORIENTED_EDGE('',*,*,#2295,.T.);
#3137=ORIENTED_EDGE('',*,*,#2298,.T.);
#3138=ORIENTED_EDGE('',*,*,#2301,.T.);
#3139=ORIENTED_EDGE('',*,*,#2314,.T.);
#3140=ORIENTED_EDGE('',*,*,#2315,.T.);
#3141=ORIENTED_EDGE('',*,*,#2316,.F.);
#3142=ORIENTED_EDGE('',*,*,#2317,.F.);
#3143=ORIENTED_EDGE('',*,*,#2318,.T.);
#3144=ORIENTED_EDGE('',*,*,#2317,.T.);
#3145=ORIENTED_EDGE('',*,*,#2319,.F.);
#3146=ORIENTED_EDGE('',*,*,#2320,.F.);
#3147=ORIENTED_EDGE('',*,*,#2321,.T.);
#3148=ORIENTED_EDGE('',*,*,#2320,.T.);
#3149=ORIENTED_EDGE('',*,*,#2322,.F.);
#3150=ORIENTED_EDGE('',*,*,#2323,.F.);
#3151=ORIENTED_EDGE('',*,*,#2324,.T.);
#3152=ORIENTED_EDGE('',*,*,#2323,.T.);
#3153=ORIENTED_EDGE('',*,*,#2325,.F.);
#3154=ORIENTED_EDGE('',*,*,#2315,.F.);
#3155=ORIENTED_EDGE('',*,*,#2325,.T.);
#3156=ORIENTED_EDGE('',*,*,#2322,.T.);
#3157=ORIENTED_EDGE('',*,*,#2319,.T.);
#3158=ORIENTED_EDGE('',*,*,#2316,.T.);
#3159=ORIENTED_EDGE('',*,*,#2324,.F.);
#3160=ORIENTED_EDGE('',*,*,#2314,.F.);
#3161=ORIENTED_EDGE('',*,*,#2318,.F.);
#3162=ORIENTED_EDGE('',*,*,#2321,.F.);
#3163=ORIENTED_EDGE('',*,*,#2326,.T.);
#3164=ORIENTED_EDGE('',*,*,#2327,.T.);
#3165=ORIENTED_EDGE('',*,*,#2328,.F.);
#3166=ORIENTED_EDGE('',*,*,#2329,.F.);
#3167=ORIENTED_EDGE('',*,*,#2330,.T.);
#3168=ORIENTED_EDGE('',*,*,#2329,.T.);
#3169=ORIENTED_EDGE('',*,*,#2331,.F.);
#3170=ORIENTED_EDGE('',*,*,#2332,.F.);
#3171=ORIENTED_EDGE('',*,*,#2333,.T.);
#3172=ORIENTED_EDGE('',*,*,#2332,.T.);
#3173=ORIENTED_EDGE('',*,*,#2334,.F.);
#3174=ORIENTED_EDGE('',*,*,#2327,.F.);
#3175=ORIENTED_EDGE('',*,*,#2334,.T.);
#3176=ORIENTED_EDGE('',*,*,#2331,.T.);
#3177=ORIENTED_EDGE('',*,*,#2328,.T.);
#3178=ORIENTED_EDGE('',*,*,#2333,.F.);
#3179=ORIENTED_EDGE('',*,*,#2326,.F.);
#3180=ORIENTED_EDGE('',*,*,#2330,.F.);
#3181=ORIENTED_EDGE('',*,*,#2335,.T.);
#3182=ORIENTED_EDGE('',*,*,#2336,.T.);
#3183=ORIENTED_EDGE('',*,*,#2337,.T.);
#3184=ORIENTED_EDGE('',*,*,#2338,.T.);
#3185=ORIENTED_EDGE('',*,*,#2339,.T.);
#3186=ORIENTED_EDGE('',*,*,#2340,.T.);
#3187=ORIENTED_EDGE('',*,*,#2335,.F.);
#3188=ORIENTED_EDGE('',*,*,#2341,.T.);
#3189=ORIENTED_EDGE('',*,*,#2342,.T.);
#3190=ORIENTED_EDGE('',*,*,#2343,.T.);
#3191=ORIENTED_EDGE('',*,*,#2339,.F.);
#3192=ORIENTED_EDGE('',*,*,#2344,.T.);
#3193=ORIENTED_EDGE('',*,*,#2345,.T.);
#3194=ORIENTED_EDGE('',*,*,#2346,.T.);
#3195=ORIENTED_EDGE('',*,*,#2342,.F.);
#3196=ORIENTED_EDGE('',*,*,#2347,.T.);
#3197=ORIENTED_EDGE('',*,*,#2348,.T.);
#3198=ORIENTED_EDGE('',*,*,#2349,.T.);
#3199=ORIENTED_EDGE('',*,*,#2345,.F.);
#3200=ORIENTED_EDGE('',*,*,#2350,.T.);
#3201=ORIENTED_EDGE('',*,*,#2351,.T.);
#3202=ORIENTED_EDGE('',*,*,#2352,.T.);
#3203=ORIENTED_EDGE('',*,*,#2348,.F.);
#3204=ORIENTED_EDGE('',*,*,#2353,.T.);
#3205=ORIENTED_EDGE('',*,*,#2354,.T.);
#3206=ORIENTED_EDGE('',*,*,#2355,.T.);
#3207=ORIENTED_EDGE('',*,*,#2351,.F.);
#3208=ORIENTED_EDGE('',*,*,#2356,.T.);
#3209=ORIENTED_EDGE('',*,*,#2357,.T.);
#3210=ORIENTED_EDGE('',*,*,#2358,.T.);
#3211=ORIENTED_EDGE('',*,*,#2354,.F.);
#3212=ORIENTED_EDGE('',*,*,#2359,.T.);
#3213=ORIENTED_EDGE('',*,*,#2360,.F.);
#3214=ORIENTED_EDGE('',*,*,#2361,.T.);
#3215=ORIENTED_EDGE('',*,*,#2362,.F.);
#3216=ORIENTED_EDGE('',*,*,#2363,.T.);
#3217=ORIENTED_EDGE('',*,*,#2364,.T.);
#3218=ORIENTED_EDGE('',*,*,#2365,.T.);
#3219=ORIENTED_EDGE('',*,*,#2366,.F.);
#3220=ORIENTED_EDGE('',*,*,#2367,.F.);
#3221=ORIENTED_EDGE('',*,*,#2368,.T.);
#3222=ORIENTED_EDGE('',*,*,#2369,.T.);
#3223=ORIENTED_EDGE('',*,*,#2364,.F.);
#3224=ORIENTED_EDGE('',*,*,#2370,.F.);
#3225=ORIENTED_EDGE('',*,*,#2371,.T.);
#3226=ORIENTED_EDGE('',*,*,#2372,.T.);
#3227=ORIENTED_EDGE('',*,*,#2368,.F.);
#3228=ORIENTED_EDGE('',*,*,#2373,.F.);
#3229=ORIENTED_EDGE('',*,*,#2374,.T.);
#3230=ORIENTED_EDGE('',*,*,#2375,.T.);
#3231=ORIENTED_EDGE('',*,*,#2371,.F.);
#3232=ORIENTED_EDGE('',*,*,#2376,.F.);
#3233=ORIENTED_EDGE('',*,*,#2377,.T.);
#3234=ORIENTED_EDGE('',*,*,#2378,.T.);
#3235=ORIENTED_EDGE('',*,*,#2374,.F.);
#3236=ORIENTED_EDGE('',*,*,#2379,.F.);
#3237=ORIENTED_EDGE('',*,*,#2380,.T.);
#3238=ORIENTED_EDGE('',*,*,#2381,.T.);
#3239=ORIENTED_EDGE('',*,*,#2377,.F.);
#3240=ORIENTED_EDGE('',*,*,#2382,.F.);
#3241=ORIENTED_EDGE('',*,*,#2383,.T.);
#3242=ORIENTED_EDGE('',*,*,#2384,.T.);
#3243=ORIENTED_EDGE('',*,*,#2380,.F.);
#3244=ORIENTED_EDGE('',*,*,#2385,.F.);
#3245=ORIENTED_EDGE('',*,*,#2386,.T.);
#3246=ORIENTED_EDGE('',*,*,#2387,.T.);
#3247=ORIENTED_EDGE('',*,*,#2383,.F.);
#3248=ORIENTED_EDGE('',*,*,#2388,.F.);
#3249=ORIENTED_EDGE('',*,*,#2389,.F.);
#3250=ORIENTED_EDGE('',*,*,#2390,.F.);
#3251=ORIENTED_EDGE('',*,*,#2391,.F.);
#3252=ORIENTED_EDGE('',*,*,#2392,.T.);
#3253=ORIENTED_EDGE('',*,*,#2389,.T.);
#3254=ORIENTED_EDGE('',*,*,#2393,.T.);
#3255=ORIENTED_EDGE('',*,*,#2386,.F.);
#3256=ORIENTED_EDGE('',*,*,#2394,.F.);
#3257=ORIENTED_EDGE('',*,*,#2395,.F.);
#3258=ORIENTED_EDGE('',*,*,#2365,.F.);
#3259=ORIENTED_EDGE('',*,*,#2369,.F.);
#3260=ORIENTED_EDGE('',*,*,#2372,.F.);
#3261=ORIENTED_EDGE('',*,*,#2375,.F.);
#3262=ORIENTED_EDGE('',*,*,#2378,.F.);
#3263=ORIENTED_EDGE('',*,*,#2381,.F.);
#3264=ORIENTED_EDGE('',*,*,#2384,.F.);
#3265=ORIENTED_EDGE('',*,*,#2387,.F.);
#3266=ORIENTED_EDGE('',*,*,#2393,.F.);
#3267=ORIENTED_EDGE('',*,*,#2392,.F.);
#3268=ORIENTED_EDGE('',*,*,#2396,.F.);
#3269=ORIENTED_EDGE('',*,*,#2336,.F.);
#3270=ORIENTED_EDGE('',*,*,#2340,.F.);
#3271=ORIENTED_EDGE('',*,*,#2343,.F.);
#3272=ORIENTED_EDGE('',*,*,#2346,.F.);
#3273=ORIENTED_EDGE('',*,*,#2349,.F.);
#3274=ORIENTED_EDGE('',*,*,#2352,.F.);
#3275=ORIENTED_EDGE('',*,*,#2355,.F.);
#3276=ORIENTED_EDGE('',*,*,#2358,.F.);
#3277=ORIENTED_EDGE('',*,*,#2397,.F.);
#3278=ORIENTED_EDGE('',*,*,#2363,.F.);
#3279=ORIENTED_EDGE('',*,*,#2398,.F.);
#3280=ORIENTED_EDGE('',*,*,#2361,.F.);
#3281=ORIENTED_EDGE('',*,*,#2399,.F.);
#3282=ORIENTED_EDGE('',*,*,#2359,.F.);
#3283=ORIENTED_EDGE('',*,*,#2356,.F.);
#3284=ORIENTED_EDGE('',*,*,#2353,.F.);
#3285=ORIENTED_EDGE('',*,*,#2350,.F.);
#3286=ORIENTED_EDGE('',*,*,#2347,.F.);
#3287=ORIENTED_EDGE('',*,*,#2344,.F.);
#3288=ORIENTED_EDGE('',*,*,#2341,.F.);
#3289=ORIENTED_EDGE('',*,*,#2338,.F.);
#3290=ORIENTED_EDGE('',*,*,#2400,.F.);
#3291=ORIENTED_EDGE('',*,*,#2390,.T.);
#3292=ORIENTED_EDGE('',*,*,#2394,.T.);
#3293=ORIENTED_EDGE('',*,*,#2388,.T.);
#3294=ORIENTED_EDGE('',*,*,#2385,.T.);
#3295=ORIENTED_EDGE('',*,*,#2382,.T.);
#3296=ORIENTED_EDGE('',*,*,#2379,.T.);
#3297=ORIENTED_EDGE('',*,*,#2376,.T.);
#3298=ORIENTED_EDGE('',*,*,#2373,.T.);
#3299=ORIENTED_EDGE('',*,*,#2370,.T.);
#3300=ORIENTED_EDGE('',*,*,#2367,.T.);
#3301=ORIENTED_EDGE('',*,*,#2401,.T.);
#3302=ORIENTED_EDGE('',*,*,#2398,.T.);
#3303=ORIENTED_EDGE('',*,*,#2366,.T.);
#3304=ORIENTED_EDGE('',*,*,#2395,.T.);
#3305=ORIENTED_EDGE('',*,*,#2362,.T.);
#3306=ORIENTED_EDGE('',*,*,#2402,.T.);
#3307=ORIENTED_EDGE('',*,*,#2403,.F.);
#3308=ORIENTED_EDGE('',*,*,#2404,.F.);
#3309=ORIENTED_EDGE('',*,*,#2405,.F.);
#3310=ORIENTED_EDGE('',*,*,#2402,.F.);
#3311=ORIENTED_EDGE('',*,*,#2406,.T.);
#3312=ORIENTED_EDGE('',*,*,#2404,.T.);
#3313=ORIENTED_EDGE('',*,*,#2406,.F.);
#3314=ORIENTED_EDGE('',*,*,#2405,.T.);
#3315=ORIENTED_EDGE('',*,*,#2407,.T.);
#3316=ORIENTED_EDGE('',*,*,#2408,.T.);
#3317=ORIENTED_EDGE('',*,*,#2407,.F.);
#3318=ORIENTED_EDGE('',*,*,#2409,.F.);
#3319=ORIENTED_EDGE('',*,*,#2410,.T.);
#3320=ORIENTED_EDGE('',*,*,#2401,.F.);
#3321=ORIENTED_EDGE('',*,*,#2411,.T.);
#3322=ORIENTED_EDGE('',*,*,#2409,.T.);
#3323=ORIENTED_EDGE('',*,*,#2411,.F.);
#3324=ORIENTED_EDGE('',*,*,#2360,.T.);
#3325=ORIENTED_EDGE('',*,*,#2397,.T.);
#3326=ORIENTED_EDGE('',*,*,#2357,.F.);
#3327=ORIENTED_EDGE('',*,*,#2399,.T.);
#3328=ORIENTED_EDGE('',*,*,#2410,.F.);
#3329=ORIENTED_EDGE('',*,*,#2412,.T.);
#3330=ORIENTED_EDGE('',*,*,#2403,.T.);
#3331=ORIENTED_EDGE('',*,*,#2412,.F.);
#3332=ORIENTED_EDGE('',*,*,#2408,.F.);
#3333=ORIENTED_EDGE('',*,*,#2400,.T.);
#3334=ORIENTED_EDGE('',*,*,#2337,.F.);
#3335=ORIENTED_EDGE('',*,*,#2396,.T.);
#3336=ORIENTED_EDGE('',*,*,#2391,.T.);
#3337=ORIENTED_EDGE('',*,*,#2413,.F.);
#3338=ORIENTED_EDGE('',*,*,#2414,.T.);
#3339=ORIENTED_EDGE('',*,*,#2415,.T.);
#3340=ORIENTED_EDGE('',*,*,#2416,.T.);
#3341=ORIENTED_EDGE('',*,*,#2417,.F.);
#3342=ORIENTED_EDGE('',*,*,#2418,.T.);
#3343=ORIENTED_EDGE('',*,*,#2413,.T.);
#3344=ORIENTED_EDGE('',*,*,#2419,.T.);
#3345=ORIENTED_EDGE('',*,*,#2420,.F.);
#3346=ORIENTED_EDGE('',*,*,#2421,.T.);
#3347=ORIENTED_EDGE('',*,*,#2417,.T.);
#3348=ORIENTED_EDGE('',*,*,#2422,.T.);
#3349=ORIENTED_EDGE('',*,*,#2423,.F.);
#3350=ORIENTED_EDGE('',*,*,#2424,.T.);
#3351=ORIENTED_EDGE('',*,*,#2420,.T.);
#3352=ORIENTED_EDGE('',*,*,#2425,.T.);
#3353=ORIENTED_EDGE('',*,*,#2426,.F.);
#3354=ORIENTED_EDGE('',*,*,#2427,.T.);
#3355=ORIENTED_EDGE('',*,*,#2423,.T.);
#3356=ORIENTED_EDGE('',*,*,#2428,.T.);
#3357=ORIENTED_EDGE('',*,*,#2429,.F.);
#3358=ORIENTED_EDGE('',*,*,#2430,.T.);
#3359=ORIENTED_EDGE('',*,*,#2426,.T.);
#3360=ORIENTED_EDGE('',*,*,#2431,.T.);
#3361=ORIENTED_EDGE('',*,*,#2432,.F.);
#3362=ORIENTED_EDGE('',*,*,#2433,.T.);
#3363=ORIENTED_EDGE('',*,*,#2429,.T.);
#3364=ORIENTED_EDGE('',*,*,#2434,.T.);
#3365=ORIENTED_EDGE('',*,*,#2435,.F.);
#3366=ORIENTED_EDGE('',*,*,#2436,.T.);
#3367=ORIENTED_EDGE('',*,*,#2432,.T.);
#3368=ORIENTED_EDGE('',*,*,#2437,.T.);
#3369=ORIENTED_EDGE('',*,*,#2438,.F.);
#3370=ORIENTED_EDGE('',*,*,#2439,.T.);
#3371=ORIENTED_EDGE('',*,*,#2435,.T.);
#3372=ORIENTED_EDGE('',*,*,#2440,.T.);
#3373=ORIENTED_EDGE('',*,*,#2441,.F.);
#3374=ORIENTED_EDGE('',*,*,#2442,.T.);
#3375=ORIENTED_EDGE('',*,*,#2438,.T.);
#3376=ORIENTED_EDGE('',*,*,#2443,.T.);
#3377=ORIENTED_EDGE('',*,*,#2444,.F.);
#3378=ORIENTED_EDGE('',*,*,#2445,.T.);
#3379=ORIENTED_EDGE('',*,*,#2441,.T.);
#3380=ORIENTED_EDGE('',*,*,#2446,.T.);
#3381=ORIENTED_EDGE('',*,*,#2447,.F.);
#3382=ORIENTED_EDGE('',*,*,#2448,.T.);
#3383=ORIENTED_EDGE('',*,*,#2449,.T.);
#3384=ORIENTED_EDGE('',*,*,#2450,.F.);
#3385=ORIENTED_EDGE('',*,*,#2451,.F.);
#3386=ORIENTED_EDGE('',*,*,#2452,.T.);
#3387=ORIENTED_EDGE('',*,*,#2447,.T.);
#3388=ORIENTED_EDGE('',*,*,#2453,.F.);
#3389=ORIENTED_EDGE('',*,*,#2454,.F.);
#3390=ORIENTED_EDGE('',*,*,#2455,.T.);
#3391=ORIENTED_EDGE('',*,*,#2451,.T.);
#3392=ORIENTED_EDGE('',*,*,#2456,.F.);
#3393=ORIENTED_EDGE('',*,*,#2457,.F.);
#3394=ORIENTED_EDGE('',*,*,#2458,.T.);
#3395=ORIENTED_EDGE('',*,*,#2454,.T.);
#3396=ORIENTED_EDGE('',*,*,#2459,.F.);
#3397=ORIENTED_EDGE('',*,*,#2460,.F.);
#3398=ORIENTED_EDGE('',*,*,#2461,.T.);
#3399=ORIENTED_EDGE('',*,*,#2457,.T.);
#3400=ORIENTED_EDGE('',*,*,#2462,.F.);
#3401=ORIENTED_EDGE('',*,*,#2463,.F.);
#3402=ORIENTED_EDGE('',*,*,#2464,.T.);
#3403=ORIENTED_EDGE('',*,*,#2460,.T.);
#3404=ORIENTED_EDGE('',*,*,#2465,.F.);
#3405=ORIENTED_EDGE('',*,*,#2466,.F.);
#3406=ORIENTED_EDGE('',*,*,#2467,.T.);
#3407=ORIENTED_EDGE('',*,*,#2463,.T.);
#3408=ORIENTED_EDGE('',*,*,#2468,.F.);
#3409=ORIENTED_EDGE('',*,*,#2469,.F.);
#3410=ORIENTED_EDGE('',*,*,#2470,.T.);
#3411=ORIENTED_EDGE('',*,*,#2466,.T.);
#3412=ORIENTED_EDGE('',*,*,#2471,.F.);
#3413=ORIENTED_EDGE('',*,*,#2472,.F.);
#3414=ORIENTED_EDGE('',*,*,#2473,.T.);
#3415=ORIENTED_EDGE('',*,*,#2469,.T.);
#3416=ORIENTED_EDGE('',*,*,#2474,.F.);
#3417=ORIENTED_EDGE('',*,*,#2475,.F.);
#3418=ORIENTED_EDGE('',*,*,#2476,.T.);
#3419=ORIENTED_EDGE('',*,*,#2472,.T.);
#3420=ORIENTED_EDGE('',*,*,#2477,.F.);
#3421=ORIENTED_EDGE('',*,*,#2478,.F.);
#3422=ORIENTED_EDGE('',*,*,#2479,.T.);
#3423=ORIENTED_EDGE('',*,*,#2475,.T.);
#3424=ORIENTED_EDGE('',*,*,#2480,.F.);
#3425=ORIENTED_EDGE('',*,*,#2481,.F.);
#3426=ORIENTED_EDGE('',*,*,#2449,.F.);
#3427=ORIENTED_EDGE('',*,*,#2482,.F.);
#3428=ORIENTED_EDGE('',*,*,#2483,.F.);
#3429=ORIENTED_EDGE('',*,*,#2484,.F.);
#3430=ORIENTED_EDGE('',*,*,#2485,.T.);
#3431=ORIENTED_EDGE('',*,*,#2486,.F.);
#3432=ORIENTED_EDGE('',*,*,#2485,.F.);
#3433=ORIENTED_EDGE('',*,*,#2482,.T.);
#3434=ORIENTED_EDGE('',*,*,#2448,.F.);
#3435=ORIENTED_EDGE('',*,*,#2452,.F.);
#3436=ORIENTED_EDGE('',*,*,#2455,.F.);
#3437=ORIENTED_EDGE('',*,*,#2458,.F.);
#3438=ORIENTED_EDGE('',*,*,#2461,.F.);
#3439=ORIENTED_EDGE('',*,*,#2464,.F.);
#3440=ORIENTED_EDGE('',*,*,#2467,.F.);
#3441=ORIENTED_EDGE('',*,*,#2470,.F.);
#3442=ORIENTED_EDGE('',*,*,#2473,.F.);
#3443=ORIENTED_EDGE('',*,*,#2476,.F.);
#3444=ORIENTED_EDGE('',*,*,#2479,.F.);
#3445=ORIENTED_EDGE('',*,*,#2487,.F.);
#3446=ORIENTED_EDGE('',*,*,#2488,.F.);
#3447=ORIENTED_EDGE('',*,*,#2414,.F.);
#3448=ORIENTED_EDGE('',*,*,#2418,.F.);
#3449=ORIENTED_EDGE('',*,*,#2421,.F.);
#3450=ORIENTED_EDGE('',*,*,#2424,.F.);
#3451=ORIENTED_EDGE('',*,*,#2427,.F.);
#3452=ORIENTED_EDGE('',*,*,#2430,.F.);
#3453=ORIENTED_EDGE('',*,*,#2433,.F.);
#3454=ORIENTED_EDGE('',*,*,#2436,.F.);
#3455=ORIENTED_EDGE('',*,*,#2439,.F.);
#3456=ORIENTED_EDGE('',*,*,#2442,.F.);
#3457=ORIENTED_EDGE('',*,*,#2445,.F.);
#3458=ORIENTED_EDGE('',*,*,#2489,.F.);
#3459=ORIENTED_EDGE('',*,*,#2478,.T.);
#3460=ORIENTED_EDGE('',*,*,#2490,.F.);
#3461=ORIENTED_EDGE('',*,*,#2491,.F.);
#3462=ORIENTED_EDGE('',*,*,#2487,.T.);
#3463=ORIENTED_EDGE('',*,*,#2481,.T.);
#3464=ORIENTED_EDGE('',*,*,#2484,.T.);
#3465=ORIENTED_EDGE('',*,*,#2492,.F.);
#3466=ORIENTED_EDGE('',*,*,#2446,.F.);
#3467=ORIENTED_EDGE('',*,*,#2443,.F.);
#3468=ORIENTED_EDGE('',*,*,#2440,.F.);
#3469=ORIENTED_EDGE('',*,*,#2437,.F.);
#3470=ORIENTED_EDGE('',*,*,#2434,.F.);
#3471=ORIENTED_EDGE('',*,*,#2431,.F.);
#3472=ORIENTED_EDGE('',*,*,#2428,.F.);
#3473=ORIENTED_EDGE('',*,*,#2425,.F.);
#3474=ORIENTED_EDGE('',*,*,#2422,.F.);
#3475=ORIENTED_EDGE('',*,*,#2419,.F.);
#3476=ORIENTED_EDGE('',*,*,#2416,.F.);
#3477=ORIENTED_EDGE('',*,*,#2493,.F.);
#3478=ORIENTED_EDGE('',*,*,#2490,.T.);
#3479=ORIENTED_EDGE('',*,*,#2480,.T.);
#3480=ORIENTED_EDGE('',*,*,#2477,.T.);
#3481=ORIENTED_EDGE('',*,*,#2474,.T.);
#3482=ORIENTED_EDGE('',*,*,#2471,.T.);
#3483=ORIENTED_EDGE('',*,*,#2468,.T.);
#3484=ORIENTED_EDGE('',*,*,#2465,.T.);
#3485=ORIENTED_EDGE('',*,*,#2462,.T.);
#3486=ORIENTED_EDGE('',*,*,#2459,.T.);
#3487=ORIENTED_EDGE('',*,*,#2456,.T.);
#3488=ORIENTED_EDGE('',*,*,#2453,.T.);
#3489=ORIENTED_EDGE('',*,*,#2450,.T.);
#3490=ORIENTED_EDGE('',*,*,#2444,.T.);
#3491=ORIENTED_EDGE('',*,*,#2492,.T.);
#3492=ORIENTED_EDGE('',*,*,#2483,.T.);
#3493=ORIENTED_EDGE('',*,*,#2489,.T.);
#3494=ORIENTED_EDGE('',*,*,#2494,.F.);
#3495=ORIENTED_EDGE('',*,*,#2495,.T.);
#3496=ORIENTED_EDGE('',*,*,#2496,.T.);
#3497=ORIENTED_EDGE('',*,*,#2497,.F.);
#3498=ORIENTED_EDGE('',*,*,#2498,.F.);
#3499=ORIENTED_EDGE('',*,*,#2499,.T.);
#3500=ORIENTED_EDGE('',*,*,#2500,.T.);
#3501=ORIENTED_EDGE('',*,*,#2495,.F.);
#3502=ORIENTED_EDGE('',*,*,#2501,.F.);
#3503=ORIENTED_EDGE('',*,*,#2502,.T.);
#3504=ORIENTED_EDGE('',*,*,#2503,.T.);
#3505=ORIENTED_EDGE('',*,*,#2499,.F.);
#3506=ORIENTED_EDGE('',*,*,#2504,.F.);
#3507=ORIENTED_EDGE('',*,*,#2505,.T.);
#3508=ORIENTED_EDGE('',*,*,#2506,.T.);
#3509=ORIENTED_EDGE('',*,*,#2502,.F.);
#3510=ORIENTED_EDGE('',*,*,#2507,.F.);
#3511=ORIENTED_EDGE('',*,*,#2508,.T.);
#3512=ORIENTED_EDGE('',*,*,#2509,.T.);
#3513=ORIENTED_EDGE('',*,*,#2505,.F.);
#3514=ORIENTED_EDGE('',*,*,#2510,.F.);
#3515=ORIENTED_EDGE('',*,*,#2497,.T.);
#3516=ORIENTED_EDGE('',*,*,#2511,.T.);
#3517=ORIENTED_EDGE('',*,*,#2508,.F.);
#3518=ORIENTED_EDGE('',*,*,#2511,.F.);
#3519=ORIENTED_EDGE('',*,*,#2496,.F.);
#3520=ORIENTED_EDGE('',*,*,#2500,.F.);
#3521=ORIENTED_EDGE('',*,*,#2503,.F.);
#3522=ORIENTED_EDGE('',*,*,#2506,.F.);
#3523=ORIENTED_EDGE('',*,*,#2509,.F.);
#3524=ORIENTED_EDGE('',*,*,#2512,.T.);
#3525=ORIENTED_EDGE('',*,*,#2488,.T.);
#3526=ORIENTED_EDGE('',*,*,#2491,.T.);
#3527=ORIENTED_EDGE('',*,*,#2493,.T.);
#3528=ORIENTED_EDGE('',*,*,#2415,.F.);
#3529=ORIENTED_EDGE('',*,*,#2512,.F.);
#3530=ORIENTED_EDGE('',*,*,#2513,.T.);
#3531=ORIENTED_EDGE('',*,*,#2514,.T.);
#3532=ORIENTED_EDGE('',*,*,#2513,.F.);
#3533=ORIENTED_EDGE('',*,*,#2514,.F.);
#3534=ORIENTED_EDGE('',*,*,#2494,.T.);
#3535=ORIENTED_EDGE('',*,*,#2510,.T.);
#3536=ORIENTED_EDGE('',*,*,#2507,.T.);
#3537=ORIENTED_EDGE('',*,*,#2504,.T.);
#3538=ORIENTED_EDGE('',*,*,#2501,.T.);
#3539=ORIENTED_EDGE('',*,*,#2498,.T.);
#3540=ORIENTED_EDGE('',*,*,#2486,.T.);
#3541=CYLINDRICAL_SURFACE('',#3975,1.);
#3542=CYLINDRICAL_SURFACE('',#3987,1.);
#3543=CYLINDRICAL_SURFACE('',#3990,1.);
#3544=CYLINDRICAL_SURFACE('',#3992,1.);
#3545=CYLINDRICAL_SURFACE('',#3994,1.);
#3546=CYLINDRICAL_SURFACE('',#3997,1.);
#3547=CYLINDRICAL_SURFACE('',#4000,1.);
#3548=CYLINDRICAL_SURFACE('',#4003,1.);
#3549=CYLINDRICAL_SURFACE('',#4010,5.);
#3550=CYLINDRICAL_SURFACE('',#4013,5.);
#3551=CYLINDRICAL_SURFACE('',#4016,1.);
#3552=CYLINDRICAL_SURFACE('',#4028,1.);
#3553=CYLINDRICAL_SURFACE('',#4031,1.);
#3554=CYLINDRICAL_SURFACE('',#4033,1.);
#3555=CYLINDRICAL_SURFACE('',#4035,1.);
#3556=CYLINDRICAL_SURFACE('',#4038,1.);
#3557=CYLINDRICAL_SURFACE('',#4041,1.);
#3558=CYLINDRICAL_SURFACE('',#4044,1.);
#3559=CYLINDRICAL_SURFACE('',#4051,1.);
#3560=CYLINDRICAL_SURFACE('',#4063,1.);
#3561=CYLINDRICAL_SURFACE('',#4066,1.);
#3562=CYLINDRICAL_SURFACE('',#4068,1.);
#3563=CYLINDRICAL_SURFACE('',#4070,1.);
#3564=CYLINDRICAL_SURFACE('',#4073,1.);
#3565=CYLINDRICAL_SURFACE('',#4076,1.);
#3566=CYLINDRICAL_SURFACE('',#4079,1.);
#3567=CYLINDRICAL_SURFACE('',#4086,4.5);
#3568=CYLINDRICAL_SURFACE('',#4089,4.5);
#3569=CYLINDRICAL_SURFACE('',#4092,1.);
#3570=CYLINDRICAL_SURFACE('',#4104,1.);
#3571=CYLINDRICAL_SURFACE('',#4106,1.);
#3572=CYLINDRICAL_SURFACE('',#4109,1.);
#3573=CYLINDRICAL_SURFACE('',#4111,1.);
#3574=CYLINDRICAL_SURFACE('',#4114,1.);
#3575=CYLINDRICAL_SURFACE('',#4117,1.);
#3576=CYLINDRICAL_SURFACE('',#4119,1.);
#3577=CYLINDRICAL_SURFACE('',#4127,3.5);
#3578=CYLINDRICAL_SURFACE('',#4130,3.5);
#3579=CYLINDRICAL_SURFACE('',#4133,3.5);
#3580=CYLINDRICAL_SURFACE('',#4136,3.5);
#3581=CYLINDRICAL_SURFACE('',#4139,3.5);
#3582=CYLINDRICAL_SURFACE('',#4142,3.5);
#3583=CYLINDRICAL_SURFACE('',#4145,3.5);
#3584=CYLINDRICAL_SURFACE('',#4148,3.5);
#3585=CYLINDRICAL_SURFACE('',#4166,7.);
#3586=CYLINDRICAL_SURFACE('',#4169,7.);
#3587=CYLINDRICAL_SURFACE('',#4172,7.);
#3588=CYLINDRICAL_SURFACE('',#4175,7.);
#3589=CYLINDRICAL_SURFACE('',#4185,7.);
#3590=CYLINDRICAL_SURFACE('',#4188,7.);
#3591=CYLINDRICAL_SURFACE('',#4191,7.);
#3592=CYLINDRICAL_SURFACE('',#4194,7.);
#3593=CYLINDRICAL_SURFACE('',#4217,2.5175);
#3594=CYLINDRICAL_SURFACE('',#4219,2.5175);
#3595=CYLINDRICAL_SURFACE('',#4220,2.5175);
#3596=CYLINDRICAL_SURFACE('',#4221,2.5175);
#3597=CYLINDRICAL_SURFACE('',#4222,2.5175);
#3598=CYLINDRICAL_SURFACE('',#4223,2.5175);
#3599=CYLINDRICAL_SURFACE('',#4224,2.5175);
#3600=CYLINDRICAL_SURFACE('',#4225,2.5175);
#3601=CYLINDRICAL_SURFACE('',#4226,2.5175);
#3602=CYLINDRICAL_SURFACE('',#4228,3.0735);
#3603=CYLINDRICAL_SURFACE('',#4230,3.0735);
#3604=CYLINDRICAL_SURFACE('',#4231,3.0735);
#3605=CYLINDRICAL_SURFACE('',#4232,3.0735);
#3606=CYLINDRICAL_SURFACE('',#4233,3.0735);
#3607=CYLINDRICAL_SURFACE('',#4234,3.0735);
#3608=CYLINDRICAL_SURFACE('',#4235,3.0735);
#3609=CYLINDRICAL_SURFACE('',#4236,3.0735);
#3610=CYLINDRICAL_SURFACE('',#4237,3.0735);
#3611=CYLINDRICAL_SURFACE('',#4239,3.0735);
#3612=CYLINDRICAL_SURFACE('',#4248,7.);
#3613=CYLINDRICAL_SURFACE('',#4249,5.);
#3614=CYLINDRICAL_SURFACE('',#4254,7.);
#3615=CYLINDRICAL_SURFACE('',#4255,2.5175);
#3616=CYLINDRICAL_SURFACE('',#4256,5.);
#3617=CYLINDRICAL_SURFACE('',#4259,2.942);
#3618=CYLINDRICAL_SURFACE('',#4261,2.942);
#3619=CYLINDRICAL_SURFACE('',#4262,2.942);
#3620=CYLINDRICAL_SURFACE('',#4263,2.942);
#3621=CYLINDRICAL_SURFACE('',#4264,2.942);
#3622=CYLINDRICAL_SURFACE('',#4265,2.942);
#3623=CYLINDRICAL_SURFACE('',#4266,2.942);
#3624=CYLINDRICAL_SURFACE('',#4267,2.942);
#3625=CYLINDRICAL_SURFACE('',#4268,2.942);
#3626=CYLINDRICAL_SURFACE('',#4269,2.942);
#3627=CYLINDRICAL_SURFACE('',#4270,2.942);
#3628=CYLINDRICAL_SURFACE('',#4271,2.37175);
#3629=CYLINDRICAL_SURFACE('',#4273,2.37175);
#3630=CYLINDRICAL_SURFACE('',#4274,2.37175);
#3631=CYLINDRICAL_SURFACE('',#4275,2.37175);
#3632=CYLINDRICAL_SURFACE('',#4276,2.37175);
#3633=CYLINDRICAL_SURFACE('',#4277,2.37175);
#3634=CYLINDRICAL_SURFACE('',#4278,2.37175);
#3635=CYLINDRICAL_SURFACE('',#4279,2.37175);
#3636=CYLINDRICAL_SURFACE('',#4280,2.37175);
#3637=CYLINDRICAL_SURFACE('',#4281,2.37175);
#3638=CYLINDRICAL_SURFACE('',#4282,2.37175);
#3639=CYLINDRICAL_SURFACE('',#4286,2.37175);
#3640=CYLINDRICAL_SURFACE('',#4288,2.942);
#3641=CYLINDRICAL_SURFACE('',#4298,5.);
#3642=ADVANCED_FACE('',(#502),#3541,.T.);
#3643=ADVANCED_FACE('',(#503),#410,.T.);
#3644=ADVANCED_FACE('',(#504,#357),#411,.T.);
#3645=ADVANCED_FACE('',(#505),#3542,.T.);
#3646=ADVANCED_FACE('',(#506),#412,.T.);
#3647=ADVANCED_FACE('',(#507),#3543,.T.);
#3648=ADVANCED_FACE('',(#508),#3544,.T.);
#3649=ADVANCED_FACE('',(#509),#3545,.F.);
#3650=ADVANCED_FACE('',(#510),#413,.T.);
#3651=ADVANCED_FACE('',(#511),#3546,.F.);
#3652=ADVANCED_FACE('',(#512),#414,.T.);
#3653=ADVANCED_FACE('',(#513),#3547,.F.);
#3654=ADVANCED_FACE('',(#514),#415,.T.);
#3655=ADVANCED_FACE('',(#515),#3548,.F.);
#3656=ADVANCED_FACE('',(#516),#416,.T.);
#3657=ADVANCED_FACE('',(#517),#417,.T.);
#3658=ADVANCED_FACE('',(#518),#418,.T.);
#3659=ADVANCED_FACE('',(#519,#358),#419,.F.);
#3660=ADVANCED_FACE('',(#520),#3549,.F.);
#3661=ADVANCED_FACE('',(#521),#3550,.F.);
#3662=ADVANCED_FACE('',(#522),#3551,.T.);
#3663=ADVANCED_FACE('',(#523),#420,.T.);
#3664=ADVANCED_FACE('',(#524,#359),#421,.T.);
#3665=ADVANCED_FACE('',(#525),#3552,.T.);
#3666=ADVANCED_FACE('',(#526),#422,.T.);
#3667=ADVANCED_FACE('',(#527),#3553,.T.);
#3668=ADVANCED_FACE('',(#528),#3554,.T.);
#3669=ADVANCED_FACE('',(#529),#3555,.F.);
#3670=ADVANCED_FACE('',(#530,#360,#361),#423,.T.);
#3671=ADVANCED_FACE('',(#531),#3556,.F.);
#3672=ADVANCED_FACE('',(#532),#424,.T.);
#3673=ADVANCED_FACE('',(#533),#3557,.F.);
#3674=ADVANCED_FACE('',(#534),#425,.T.);
#3675=ADVANCED_FACE('',(#535),#3558,.F.);
#3676=ADVANCED_FACE('',(#536),#426,.T.);
#3677=ADVANCED_FACE('',(#537,#362,#363),#427,.T.);
#3678=ADVANCED_FACE('',(#538),#428,.T.);
#3679=ADVANCED_FACE('',(#539,#364),#429,.F.);
#3680=ADVANCED_FACE('',(#540),#3559,.T.);
#3681=ADVANCED_FACE('',(#541),#430,.T.);
#3682=ADVANCED_FACE('',(#542,#365),#431,.T.);
#3683=ADVANCED_FACE('',(#543),#3560,.T.);
#3684=ADVANCED_FACE('',(#544),#432,.T.);
#3685=ADVANCED_FACE('',(#545),#3561,.T.);
#3686=ADVANCED_FACE('',(#546),#3562,.T.);
#3687=ADVANCED_FACE('',(#547),#3563,.F.);
#3688=ADVANCED_FACE('',(#548),#433,.T.);
#3689=ADVANCED_FACE('',(#549),#3564,.F.);
#3690=ADVANCED_FACE('',(#550),#434,.T.);
#3691=ADVANCED_FACE('',(#551),#3565,.F.);
#3692=ADVANCED_FACE('',(#552),#435,.T.);
#3693=ADVANCED_FACE('',(#553),#3566,.F.);
#3694=ADVANCED_FACE('',(#554),#436,.T.);
#3695=ADVANCED_FACE('',(#555),#437,.T.);
#3696=ADVANCED_FACE('',(#556),#438,.T.);
#3697=ADVANCED_FACE('',(#557,#366),#439,.F.);
#3698=ADVANCED_FACE('',(#558),#3567,.F.);
#3699=ADVANCED_FACE('',(#559),#3568,.F.);
#3700=ADVANCED_FACE('',(#560),#3569,.T.);
#3701=ADVANCED_FACE('',(#561),#440,.T.);
#3702=ADVANCED_FACE('',(#562,#367,#368),#441,.T.);
#3703=ADVANCED_FACE('',(#563),#3570,.T.);
#3704=ADVANCED_FACE('',(#564),#3571,.T.);
#3705=ADVANCED_FACE('',(#565),#442,.T.);
#3706=ADVANCED_FACE('',(#566),#3572,.T.);
#3707=ADVANCED_FACE('',(#567),#3573,.F.);
#3708=ADVANCED_FACE('',(#568,#369,#370),#443,.T.);
#3709=ADVANCED_FACE('',(#569),#3574,.F.);
#3710=ADVANCED_FACE('',(#570),#444,.T.);
#3711=ADVANCED_FACE('',(#571),#3575,.T.);
#3712=ADVANCED_FACE('',(#572),#3576,.T.);
#3713=ADVANCED_FACE('',(#573),#445,.T.);
#3714=ADVANCED_FACE('',(#574),#446,.T.);
#3715=ADVANCED_FACE('',(#575),#447,.T.);
#3716=ADVANCED_FACE('',(#576),#448,.T.);
#3717=ADVANCED_FACE('',(#577),#449,.F.);
#3718=ADVANCED_FACE('',(#578),#3577,.F.);
#3719=ADVANCED_FACE('',(#579),#3578,.F.);
#3720=ADVANCED_FACE('',(#580),#3579,.F.);
#3721=ADVANCED_FACE('',(#581),#3580,.F.);
#3722=ADVANCED_FACE('',(#582),#3581,.F.);
#3723=ADVANCED_FACE('',(#583),#3582,.F.);
#3724=ADVANCED_FACE('',(#584),#3583,.F.);
#3725=ADVANCED_FACE('',(#585),#3584,.F.);
#3726=ADVANCED_FACE('',(#586),#450,.F.);
#3727=ADVANCED_FACE('',(#587),#451,.F.);
#3728=ADVANCED_FACE('',(#588),#452,.F.);
#3729=ADVANCED_FACE('',(#589),#453,.F.);
#3730=ADVANCED_FACE('',(#590),#454,.F.);
#3731=ADVANCED_FACE('',(#591),#455,.F.);
#3732=ADVANCED_FACE('',(#592),#456,.F.);
#3733=ADVANCED_FACE('',(#593),#457,.F.);
#3734=ADVANCED_FACE('',(#594),#458,.T.);
#3735=ADVANCED_FACE('',(#595),#459,.T.);
#3736=ADVANCED_FACE('',(#596,#371,#372,#373,#374,#375,#376,#377,#378),#460,
 .F.);
#3737=ADVANCED_FACE('',(#597,#379,#380,#381,#382,#383,#384,#385,#386),#461,
 .T.);
#3738=ADVANCED_FACE('',(#598),#462,.T.);
#3739=ADVANCED_FACE('',(#599),#463,.T.);
#3740=ADVANCED_FACE('',(#600),#3585,.F.);
#3741=ADVANCED_FACE('',(#601),#3586,.F.);
#3742=ADVANCED_FACE('',(#602),#3587,.F.);
#3743=ADVANCED_FACE('',(#603),#3588,.F.);
#3744=ADVANCED_FACE('',(#604),#464,.T.);
#3745=ADVANCED_FACE('',(#605),#465,.T.);
#3746=ADVANCED_FACE('',(#606),#466,.T.);
#3747=ADVANCED_FACE('',(#607),#467,.T.);
#3748=ADVANCED_FACE('',(#608,#387,#388,#389,#390),#468,.T.);
#3749=ADVANCED_FACE('',(#609,#391,#392,#393,#394),#469,.F.);
#3750=ADVANCED_FACE('',(#610),#3589,.F.);
#3751=ADVANCED_FACE('',(#611),#3590,.F.);
#3752=ADVANCED_FACE('',(#612),#3591,.F.);
#3753=ADVANCED_FACE('',(#613),#3592,.F.);
#3754=ADVANCED_FACE('',(#614),#470,.T.);
#3755=ADVANCED_FACE('',(#615),#471,.T.);
#3756=ADVANCED_FACE('',(#616),#472,.T.);
#3757=ADVANCED_FACE('',(#617),#473,.T.);
#3758=ADVANCED_FACE('',(#618,#395,#396,#397,#398),#474,.T.);
#3759=ADVANCED_FACE('',(#619,#399,#400,#401,#402),#475,.F.);
#3760=ADVANCED_FACE('',(#620),#476,.T.);
#3761=ADVANCED_FACE('',(#621),#477,.T.);
#3762=ADVANCED_FACE('',(#622),#478,.T.);
#3763=ADVANCED_FACE('',(#623),#479,.T.);
#3764=ADVANCED_FACE('',(#624),#480,.T.);
#3765=ADVANCED_FACE('',(#625),#481,.F.);
#3766=ADVANCED_FACE('',(#626),#482,.T.);
#3767=ADVANCED_FACE('',(#627),#483,.T.);
#3768=ADVANCED_FACE('',(#628),#484,.T.);
#3769=ADVANCED_FACE('',(#629),#485,.T.);
#3770=ADVANCED_FACE('',(#630),#486,.F.);
#3771=ADVANCED_FACE('',(#631),#3593,.F.);
#3772=ADVANCED_FACE('',(#632),#3594,.F.);
#3773=ADVANCED_FACE('',(#633),#3595,.F.);
#3774=ADVANCED_FACE('',(#634),#3596,.F.);
#3775=ADVANCED_FACE('',(#635),#3597,.F.);
#3776=ADVANCED_FACE('',(#636),#3598,.F.);
#3777=ADVANCED_FACE('',(#637),#3599,.F.);
#3778=ADVANCED_FACE('',(#638),#3600,.F.);
#3779=ADVANCED_FACE('',(#639),#3601,.F.);
#3780=ADVANCED_FACE('',(#640),#3602,.F.);
#3781=ADVANCED_FACE('',(#641),#3603,.F.);
#3782=ADVANCED_FACE('',(#642),#3604,.F.);
#3783=ADVANCED_FACE('',(#643),#3605,.F.);
#3784=ADVANCED_FACE('',(#644),#3606,.F.);
#3785=ADVANCED_FACE('',(#645),#3607,.F.);
#3786=ADVANCED_FACE('',(#646),#3608,.F.);
#3787=ADVANCED_FACE('',(#647),#3609,.F.);
#3788=ADVANCED_FACE('',(#648),#3610,.F.);
#3789=ADVANCED_FACE('',(#649),#3611,.F.);
#3790=ADVANCED_FACE('',(#650),#212,.F.);
#3791=ADVANCED_FACE('',(#651),#213,.F.);
#3792=ADVANCED_FACE('',(#652,#403),#487,.T.);
#3793=ADVANCED_FACE('',(#653,#404),#488,.T.);
#3794=ADVANCED_FACE('',(#654,#405),#489,.F.);
#3795=ADVANCED_FACE('',(#655),#3612,.T.);
#3796=ADVANCED_FACE('',(#656),#3613,.T.);
#3797=ADVANCED_FACE('',(#657,#406),#490,.F.);
#3798=ADVANCED_FACE('',(#658),#3614,.T.);
#3799=ADVANCED_FACE('',(#659),#3615,.F.);
#3800=ADVANCED_FACE('',(#660),#3616,.T.);
#3801=ADVANCED_FACE('',(#661,#407),#491,.F.);
#3802=ADVANCED_FACE('',(#662),#3617,.T.);
#3803=ADVANCED_FACE('',(#663),#3618,.T.);
#3804=ADVANCED_FACE('',(#664),#3619,.T.);
#3805=ADVANCED_FACE('',(#665),#3620,.T.);
#3806=ADVANCED_FACE('',(#666),#3621,.T.);
#3807=ADVANCED_FACE('',(#667),#3622,.T.);
#3808=ADVANCED_FACE('',(#668),#3623,.T.);
#3809=ADVANCED_FACE('',(#669),#3624,.T.);
#3810=ADVANCED_FACE('',(#670),#3625,.T.);
#3811=ADVANCED_FACE('',(#671),#3626,.T.);
#3812=ADVANCED_FACE('',(#672),#3627,.T.);
#3813=ADVANCED_FACE('',(#673),#3628,.T.);
#3814=ADVANCED_FACE('',(#674),#3629,.T.);
#3815=ADVANCED_FACE('',(#675),#3630,.T.);
#3816=ADVANCED_FACE('',(#676),#3631,.T.);
#3817=ADVANCED_FACE('',(#677),#3632,.T.);
#3818=ADVANCED_FACE('',(#678),#3633,.T.);
#3819=ADVANCED_FACE('',(#679),#3634,.T.);
#3820=ADVANCED_FACE('',(#680),#3635,.T.);
#3821=ADVANCED_FACE('',(#681),#3636,.T.);
#3822=ADVANCED_FACE('',(#682),#3637,.T.);
#3823=ADVANCED_FACE('',(#683),#3638,.T.);
#3824=ADVANCED_FACE('',(#684),#211,.T.);
#3825=ADVANCED_FACE('',(#685),#214,.F.);
#3826=ADVANCED_FACE('',(#686),#3639,.T.);
#3827=ADVANCED_FACE('',(#687),#215,.F.);
#3828=ADVANCED_FACE('',(#688),#3640,.T.);
#3829=ADVANCED_FACE('',(#689),#492,.F.);
#3830=ADVANCED_FACE('',(#690),#493,.F.);
#3831=ADVANCED_FACE('',(#691),#494,.F.);
#3832=ADVANCED_FACE('',(#692),#495,.F.);
#3833=ADVANCED_FACE('',(#693),#496,.F.);
#3834=ADVANCED_FACE('',(#694),#497,.F.);
#3835=ADVANCED_FACE('',(#695),#498,.F.);
#3836=ADVANCED_FACE('',(#696,#408),#499,.T.);
#3837=ADVANCED_FACE('',(#697),#3641,.T.);
#3838=ADVANCED_FACE('',(#698,#409),#500,.F.);
#3839=ADVANCED_FACE('',(#699),#501,.T.);
#3840=CLOSED_SHELL('',(#3642,#3643,#3644,#3645,#3646,#3647,#3648,#3649,
#3650,#3651,#3652,#3653,#3654,#3655,#3656,#3657,#3658,#3659));
#3841=CLOSED_SHELL('',(#3660,#3661,#3662,#3663,#3664,#3665,#3666,#3667,
#3668,#3669,#3670,#3671,#3672,#3673,#3674,#3675,#3676,#3677,#3678,#3679));
#3842=CLOSED_SHELL('',(#3680,#3681,#3682,#3683,#3684,#3685,#3686,#3687,
#3688,#3689,#3690,#3691,#3692,#3693,#3694,#3695,#3696,#3697));
#3843=CLOSED_SHELL('',(#3698,#3699,#3700,#3701,#3702,#3703,#3704,#3705,
#3706,#3707,#3708,#3709,#3710,#3711,#3712,#3713,#3714,#3715,#3716,#3717));
#3844=CLOSED_SHELL('',(#3718,#3719,#3720,#3721,#3722,#3723,#3724,#3725,
#3726,#3727,#3728,#3729,#3730,#3731,#3732,#3733,#3734,#3735,#3736,#3737,
#3738,#3739));
#3845=CLOSED_SHELL('',(#3740,#3741,#3742,#3743,#3744,#3745,#3746,#3747,
#3748,#3749));
#3846=CLOSED_SHELL('',(#3750,#3751,#3752,#3753,#3754,#3755,#3756,#3757,
#3758,#3759));
#3847=CLOSED_SHELL('',(#3760,#3761,#3762,#3763,#3764,#3765));
#3848=CLOSED_SHELL('',(#3766,#3767,#3768,#3769,#3770));
#3849=CLOSED_SHELL('',(#3771,#3772,#3773,#3774,#3775,#3776,#3777,#3778,
#3779,#3780,#3781,#3782,#3783,#3784,#3785,#3786,#3787,#3788,#3789,#3790,
#3791,#3792,#3793,#3794,#3795,#3796,#3797,#3798,#3799,#3800,#3801));
#3850=CLOSED_SHELL('',(#3802,#3803,#3804,#3805,#3806,#3807,#3808,#3809,
#3810,#3811,#3812,#3813,#3814,#3815,#3816,#3817,#3818,#3819,#3820,#3821,
#3822,#3823,#3824,#3825,#3826,#3827,#3828,#3829,#3830,#3831,#3832,#3833,
#3834,#3835,#3836,#3837,#3838,#3839));
#3851=DERIVED_UNIT_ELEMENT(#3873,1.);
#3852=DERIVED_UNIT_ELEMENT(#9779,-3.);
#3853=DERIVED_UNIT_ELEMENT(#3873,1.);
#3854=DERIVED_UNIT_ELEMENT(#9779,-3.);
#3855=DERIVED_UNIT_ELEMENT(#3873,1.);
#3856=DERIVED_UNIT_ELEMENT(#9779,-3.);
#3857=DERIVED_UNIT_ELEMENT(#3873,1.);
#3858=DERIVED_UNIT_ELEMENT(#9779,-3.);
#3859=DERIVED_UNIT_ELEMENT(#3873,1.);
#3860=DERIVED_UNIT_ELEMENT(#9779,-3.);
#3861=DERIVED_UNIT_ELEMENT(#3873,1.);
#3862=DERIVED_UNIT_ELEMENT(#9779,-3.);
#3863=DERIVED_UNIT_ELEMENT(#3873,1.);
#3864=DERIVED_UNIT_ELEMENT(#9779,-3.);
#3865=DERIVED_UNIT_ELEMENT(#3873,1.);
#3866=DERIVED_UNIT_ELEMENT(#9779,-3.);
#3867=DERIVED_UNIT_ELEMENT(#3873,1.);
#3868=DERIVED_UNIT_ELEMENT(#9779,-3.);
#3869=DERIVED_UNIT_ELEMENT(#3873,1.);
#3870=DERIVED_UNIT_ELEMENT(#9779,-3.);
#3871=DERIVED_UNIT_ELEMENT(#3873,1.);
#3872=DERIVED_UNIT_ELEMENT(#9779,-3.);
#3873=(
MASS_UNIT()
NAMED_UNIT(*)
SI_UNIT(.KILO.,.GRAM.)
);
#3874=DERIVED_UNIT((#3851,#3852));
#3875=DERIVED_UNIT((#3853,#3854));
#3876=DERIVED_UNIT((#3855,#3856));
#3877=DERIVED_UNIT((#3857,#3858));
#3878=DERIVED_UNIT((#3859,#3860));
#3879=DERIVED_UNIT((#3861,#3862));
#3880=DERIVED_UNIT((#3863,#3864));
#3881=DERIVED_UNIT((#3865,#3866));
#3882=DERIVED_UNIT((#3867,#3868));
#3883=DERIVED_UNIT((#3869,#3870));
#3884=DERIVED_UNIT((#3871,#3872));
#3885=MEASURE_REPRESENTATION_ITEM('density measure',
POSITIVE_RATIO_MEASURE(2700.),#3874);
#3886=MEASURE_REPRESENTATION_ITEM('density measure',
POSITIVE_RATIO_MEASURE(2700.),#3875);
#3887=MEASURE_REPRESENTATION_ITEM('density measure',
POSITIVE_RATIO_MEASURE(2700.),#3876);
#3888=MEASURE_REPRESENTATION_ITEM('density measure',
POSITIVE_RATIO_MEASURE(2700.),#3877);
#3889=MEASURE_REPRESENTATION_ITEM('density measure',
POSITIVE_RATIO_MEASURE(2700.),#3878);
#3890=MEASURE_REPRESENTATION_ITEM('density measure',
POSITIVE_RATIO_MEASURE(2700.),#3879);
#3891=MEASURE_REPRESENTATION_ITEM('density measure',
POSITIVE_RATIO_MEASURE(1200.),#3880);
#3892=MEASURE_REPRESENTATION_ITEM('density measure',
POSITIVE_RATIO_MEASURE(2700.),#3881);
#3893=MEASURE_REPRESENTATION_ITEM('density measure',
POSITIVE_RATIO_MEASURE(2700.),#3882);
#3894=MEASURE_REPRESENTATION_ITEM('density measure',
POSITIVE_RATIO_MEASURE(7850.),#3883);
#3895=MEASURE_REPRESENTATION_ITEM('density measure',
POSITIVE_RATIO_MEASURE(7850.),#3884);
#3896=PROPERTY_DEFINITION_REPRESENTATION(#3951,#3918);
#3897=PROPERTY_DEFINITION_REPRESENTATION(#3952,#3919);
#3898=PROPERTY_DEFINITION_REPRESENTATION(#3953,#3920);
#3899=PROPERTY_DEFINITION_REPRESENTATION(#3954,#3921);
#3900=PROPERTY_DEFINITION_REPRESENTATION(#3955,#3922);
#3901=PROPERTY_DEFINITION_REPRESENTATION(#3956,#3923);
#3902=PROPERTY_DEFINITION_REPRESENTATION(#3957,#3924);
#3903=PROPERTY_DEFINITION_REPRESENTATION(#3958,#3925);
#3904=PROPERTY_DEFINITION_REPRESENTATION(#3959,#3926);
#3905=PROPERTY_DEFINITION_REPRESENTATION(#3960,#3927);
#3906=PROPERTY_DEFINITION_REPRESENTATION(#3961,#3928);
#3907=PROPERTY_DEFINITION_REPRESENTATION(#3962,#3929);
#3908=PROPERTY_DEFINITION_REPRESENTATION(#3963,#3930);
#3909=PROPERTY_DEFINITION_REPRESENTATION(#3964,#3931);
#3910=PROPERTY_DEFINITION_REPRESENTATION(#3965,#3932);
#3911=PROPERTY_DEFINITION_REPRESENTATION(#3966,#3933);
#3912=PROPERTY_DEFINITION_REPRESENTATION(#3967,#3934);
#3913=PROPERTY_DEFINITION_REPRESENTATION(#3968,#3935);
#3914=PROPERTY_DEFINITION_REPRESENTATION(#3969,#3936);
#3915=PROPERTY_DEFINITION_REPRESENTATION(#3970,#3937);
#3916=PROPERTY_DEFINITION_REPRESENTATION(#3971,#3938);
#3917=PROPERTY_DEFINITION_REPRESENTATION(#3972,#3939);
#3918=REPRESENTATION('material name',(#3940),#9766);
#3919=REPRESENTATION('density',(#3885),#9766);
#3920=REPRESENTATION('material name',(#3941),#9767);
#3921=REPRESENTATION('density',(#3886),#9767);
#3922=REPRESENTATION('material name',(#3942),#9768);
#3923=REPRESENTATION('density',(#3887),#9768);
#3924=REPRESENTATION('material name',(#3943),#9769);
#3925=REPRESENTATION('density',(#3888),#9769);
#3926=REPRESENTATION('material name',(#3944),#9770);
#3927=REPRESENTATION('density',(#3889),#9770);
#3928=REPRESENTATION('material name',(#3945),#9771);
#3929=REPRESENTATION('density',(#3890),#9771);
#3930=REPRESENTATION('material name',(#3946),#9772);
#3931=REPRESENTATION('density',(#3891),#9772);
#3932=REPRESENTATION('material name',(#3947),#9773);
#3933=REPRESENTATION('density',(#3892),#9773);
#3934=REPRESENTATION('material name',(#3948),#9774);
#3935=REPRESENTATION('density',(#3893),#9774);
#3936=REPRESENTATION('material name',(#3949),#9775);
#3937=REPRESENTATION('density',(#3894),#9775);
#3938=REPRESENTATION('material name',(#3950),#9776);
#3939=REPRESENTATION('density',(#3895),#9776);
#3940=DESCRIPTIVE_REPRESENTATION_ITEM('Aluminum 6061','Aluminum 6061');
#3941=DESCRIPTIVE_REPRESENTATION_ITEM('Aluminum 6061','Aluminum 6061');
#3942=DESCRIPTIVE_REPRESENTATION_ITEM('Aluminum 6061','Aluminum 6061');
#3943=DESCRIPTIVE_REPRESENTATION_ITEM('Aluminum 6061','Aluminum 6061');
#3944=DESCRIPTIVE_REPRESENTATION_ITEM('Aluminum 6061','Aluminum 6061');
#3945=DESCRIPTIVE_REPRESENTATION_ITEM('Aluminum 6061','Aluminum 6061');
#3946=DESCRIPTIVE_REPRESENTATION_ITEM('Rubber, Nitrile',
'Rubber, Nitrile');
#3947=DESCRIPTIVE_REPRESENTATION_ITEM('Aluminum 6061','Aluminum 6061');
#3948=DESCRIPTIVE_REPRESENTATION_ITEM('Aluminum 6061','Aluminum 6061');
#3949=DESCRIPTIVE_REPRESENTATION_ITEM('Steel','Steel');
#3950=DESCRIPTIVE_REPRESENTATION_ITEM('Steel','Steel');
#3951=PROPERTY_DEFINITION('material property','material name',#9870);
#3952=PROPERTY_DEFINITION('material property','density of part',#9870);
#3953=PROPERTY_DEFINITION('material property','material name',#9871);
#3954=PROPERTY_DEFINITION('material property','density of part',#9871);
#3955=PROPERTY_DEFINITION('material property','material name',#9872);
#3956=PROPERTY_DEFINITION('material property','density of part',#9872);
#3957=PROPERTY_DEFINITION('material property','material name',#9873);
#3958=PROPERTY_DEFINITION('material property','density of part',#9873);
#3959=PROPERTY_DEFINITION('material property','material name',#9874);
#3960=PROPERTY_DEFINITION('material property','density of part',#9874);
#3961=PROPERTY_DEFINITION('material property','material name',#9875);
#3962=PROPERTY_DEFINITION('material property','density of part',#9875);
#3963=PROPERTY_DEFINITION('material property','material name',#9876);
#3964=PROPERTY_DEFINITION('material property','density of part',#9876);
#3965=PROPERTY_DEFINITION('material property','material name',#9877);
#3966=PROPERTY_DEFINITION('material property','density of part',#9877);
#3967=PROPERTY_DEFINITION('material property','material name',#9878);
#3968=PROPERTY_DEFINITION('material property','density of part',#9878);
#3969=PROPERTY_DEFINITION('material property','material name',#9879);
#3970=PROPERTY_DEFINITION('material property','density of part',#9879);
#3971=PROPERTY_DEFINITION('material property','material name',#9880);
#3972=PROPERTY_DEFINITION('material property','density of part',#9880);
#3973=AXIS2_PLACEMENT_3D('',#5403,#4352,#4353);
#3974=AXIS2_PLACEMENT_3D('',#5404,#4354,#4355);
#3975=AXIS2_PLACEMENT_3D('',#5405,#4356,#4357);
#3976=AXIS2_PLACEMENT_3D('',#5408,#4358,#4359);
#3977=AXIS2_PLACEMENT_3D('',#5412,#4361,#4362);
#3978=AXIS2_PLACEMENT_3D('',#5414,#4364,#4365);
#3979=AXIS2_PLACEMENT_3D('',#5420,#4369,#4370);
#3980=AXIS2_PLACEMENT_3D('',#5424,#4372,#4373);
#3981=AXIS2_PLACEMENT_3D('',#5428,#4375,#4376);
#3982=AXIS2_PLACEMENT_3D('',#5431,#4378,#4379);
#3983=AXIS2_PLACEMENT_3D('',#5436,#4381,#4382);
#3984=AXIS2_PLACEMENT_3D('',#5440,#4384,#4385);
#3985=AXIS2_PLACEMENT_3D('',#5444,#4387,#4388);
#3986=AXIS2_PLACEMENT_3D('',#5447,#4390,#4391);
#3987=AXIS2_PLACEMENT_3D('',#5448,#4392,#4393);
#3988=AXIS2_PLACEMENT_3D('',#5452,#4395,#4396);
#3989=AXIS2_PLACEMENT_3D('',#5454,#4398,#4399);
#3990=AXIS2_PLACEMENT_3D('',#5458,#4402,#4403);
#3991=AXIS2_PLACEMENT_3D('',#5460,#4404,#4405);
#3992=AXIS2_PLACEMENT_3D('',#5462,#4407,#4408);
#3993=AXIS2_PLACEMENT_3D('',#5465,#4410,#4411);
#3994=AXIS2_PLACEMENT_3D('',#5466,#4412,#4413);
#3995=AXIS2_PLACEMENT_3D('',#5469,#4414,#4415);
#3996=AXIS2_PLACEMENT_3D('',#5472,#4418,#4419);
#3997=AXIS2_PLACEMENT_3D('',#5476,#4422,#4423);
#3998=AXIS2_PLACEMENT_3D('',#5478,#4424,#4425);
#3999=AXIS2_PLACEMENT_3D('',#5480,#4427,#4428);
#4000=AXIS2_PLACEMENT_3D('',#5484,#4431,#4432);
#4001=AXIS2_PLACEMENT_3D('',#5486,#4433,#4434);
#4002=AXIS2_PLACEMENT_3D('',#5488,#4436,#4437);
#4003=AXIS2_PLACEMENT_3D('',#5492,#4440,#4441);
#4004=AXIS2_PLACEMENT_3D('',#5494,#4442,#4443);
#4005=AXIS2_PLACEMENT_3D('',#5496,#4445,#4446);
#4006=AXIS2_PLACEMENT_3D('',#5498,#4448,#4449);
#4007=AXIS2_PLACEMENT_3D('',#5500,#4451,#4452);
#4008=AXIS2_PLACEMENT_3D('',#5502,#4454,#4455);
#4009=AXIS2_PLACEMENT_3D('',#5503,#4456,#4457);
#4010=AXIS2_PLACEMENT_3D('',#5504,#4458,#4459);
#4011=AXIS2_PLACEMENT_3D('',#5506,#4460,#4461);
#4012=AXIS2_PLACEMENT_3D('',#5509,#4463,#4464);
#4013=AXIS2_PLACEMENT_3D('',#5510,#4465,#4466);
#4014=AXIS2_PLACEMENT_3D('',#5512,#4467,#4468);
#4015=AXIS2_PLACEMENT_3D('',#5515,#4470,#4471);
#4016=AXIS2_PLACEMENT_3D('',#5516,#4472,#4473);
#4017=AXIS2_PLACEMENT_3D('',#5519,#4474,#4475);
#4018=AXIS2_PLACEMENT_3D('',#5523,#4477,#4478);
#4019=AXIS2_PLACEMENT_3D('',#5525,#4480,#4481);
#4020=AXIS2_PLACEMENT_3D('',#5531,#4485,#4486);
#4021=AXIS2_PLACEMENT_3D('',#5535,#4488,#4489);
#4022=AXIS2_PLACEMENT_3D('',#5539,#4491,#4492);
#4023=AXIS2_PLACEMENT_3D('',#5542,#4494,#4495);
#4024=AXIS2_PLACEMENT_3D('',#5547,#4497,#4498);
#4025=AXIS2_PLACEMENT_3D('',#5551,#4500,#4501);
#4026=AXIS2_PLACEMENT_3D('',#5555,#4503,#4504);
#4027=AXIS2_PLACEMENT_3D('',#5558,#4506,#4507);
#4028=AXIS2_PLACEMENT_3D('',#5559,#4508,#4509);
#4029=AXIS2_PLACEMENT_3D('',#5563,#4511,#4512);
#4030=AXIS2_PLACEMENT_3D('',#5565,#4514,#4515);
#4031=AXIS2_PLACEMENT_3D('',#5569,#4518,#4519);
#4032=AXIS2_PLACEMENT_3D('',#5571,#4520,#4521);
#4033=AXIS2_PLACEMENT_3D('',#5573,#4523,#4524);
#4034=AXIS2_PLACEMENT_3D('',#5576,#4526,#4527);
#4035=AXIS2_PLACEMENT_3D('',#5577,#4528,#4529);
#4036=AXIS2_PLACEMENT_3D('',#5580,#4530,#4531);
#4037=AXIS2_PLACEMENT_3D('',#5583,#4534,#4535);
#4038=AXIS2_PLACEMENT_3D('',#5587,#4538,#4539);
#4039=AXIS2_PLACEMENT_3D('',#5589,#4540,#4541);
#4040=AXIS2_PLACEMENT_3D('',#5591,#4543,#4544);
#4041=AXIS2_PLACEMENT_3D('',#5595,#4547,#4548);
#4042=AXIS2_PLACEMENT_3D('',#5597,#4549,#4550);
#4043=AXIS2_PLACEMENT_3D('',#5599,#4552,#4553);
#4044=AXIS2_PLACEMENT_3D('',#5603,#4556,#4557);
#4045=AXIS2_PLACEMENT_3D('',#5605,#4558,#4559);
#4046=AXIS2_PLACEMENT_3D('',#5607,#4561,#4562);
#4047=AXIS2_PLACEMENT_3D('',#5609,#4564,#4565);
#4048=AXIS2_PLACEMENT_3D('',#5611,#4567,#4568);
#4049=AXIS2_PLACEMENT_3D('',#5613,#4570,#4571);
#4050=AXIS2_PLACEMENT_3D('',#5614,#4572,#4573);
#4051=AXIS2_PLACEMENT_3D('',#5615,#4574,#4575);
#4052=AXIS2_PLACEMENT_3D('',#5618,#4576,#4577);
#4053=AXIS2_PLACEMENT_3D('',#5622,#4579,#4580);
#4054=AXIS2_PLACEMENT_3D('',#5624,#4582,#4583);
#4055=AXIS2_PLACEMENT_3D('',#5630,#4587,#4588);
#4056=AXIS2_PLACEMENT_3D('',#5634,#4590,#4591);
#4057=AXIS2_PLACEMENT_3D('',#5638,#4593,#4594);
#4058=AXIS2_PLACEMENT_3D('',#5641,#4596,#4597);
#4059=AXIS2_PLACEMENT_3D('',#5646,#4599,#4600);
#4060=AXIS2_PLACEMENT_3D('',#5650,#4602,#4603);
#4061=AXIS2_PLACEMENT_3D('',#5654,#4605,#4606);
#4062=AXIS2_PLACEMENT_3D('',#5657,#4608,#4609);
#4063=AXIS2_PLACEMENT_3D('',#5658,#4610,#4611);
#4064=AXIS2_PLACEMENT_3D('',#5662,#4613,#4614);
#4065=AXIS2_PLACEMENT_3D('',#5664,#4616,#4617);
#4066=AXIS2_PLACEMENT_3D('',#5668,#4620,#4621);
#4067=AXIS2_PLACEMENT_3D('',#5670,#4622,#4623);
#4068=AXIS2_PLACEMENT_3D('',#5672,#4625,#4626);
#4069=AXIS2_PLACEMENT_3D('',#5675,#4628,#4629);
#4070=AXIS2_PLACEMENT_3D('',#5676,#4630,#4631);
#4071=AXIS2_PLACEMENT_3D('',#5679,#4632,#4633);
#4072=AXIS2_PLACEMENT_3D('',#5682,#4636,#4637);
#4073=AXIS2_PLACEMENT_3D('',#5686,#4640,#4641);
#4074=AXIS2_PLACEMENT_3D('',#5688,#4642,#4643);
#4075=AXIS2_PLACEMENT_3D('',#5690,#4645,#4646);
#4076=AXIS2_PLACEMENT_3D('',#5694,#4649,#4650);
#4077=AXIS2_PLACEMENT_3D('',#5696,#4651,#4652);
#4078=AXIS2_PLACEMENT_3D('',#5698,#4654,#4655);
#4079=AXIS2_PLACEMENT_3D('',#5702,#4658,#4659);
#4080=AXIS2_PLACEMENT_3D('',#5704,#4660,#4661);
#4081=AXIS2_PLACEMENT_3D('',#5706,#4663,#4664);
#4082=AXIS2_PLACEMENT_3D('',#5708,#4666,#4667);
#4083=AXIS2_PLACEMENT_3D('',#5710,#4669,#4670);
#4084=AXIS2_PLACEMENT_3D('',#5712,#4672,#4673);
#4085=AXIS2_PLACEMENT_3D('',#5713,#4674,#4675);
#4086=AXIS2_PLACEMENT_3D('',#5714,#4676,#4677);
#4087=AXIS2_PLACEMENT_3D('',#5716,#4678,#4679);
#4088=AXIS2_PLACEMENT_3D('',#5719,#4681,#4682);
#4089=AXIS2_PLACEMENT_3D('',#5720,#4683,#4684);
#4090=AXIS2_PLACEMENT_3D('',#5722,#4685,#4686);
#4091=AXIS2_PLACEMENT_3D('',#5725,#4688,#4689);
#4092=AXIS2_PLACEMENT_3D('',#5726,#4690,#4691);
#4093=AXIS2_PLACEMENT_3D('',#5729,#4692,#4693);
#4094=AXIS2_PLACEMENT_3D('',#5733,#4695,#4696);
#4095=AXIS2_PLACEMENT_3D('',#5735,#4698,#4699);
#4096=AXIS2_PLACEMENT_3D('',#5739,#4701,#4702);
#4097=AXIS2_PLACEMENT_3D('',#5743,#4704,#4705);
#4098=AXIS2_PLACEMENT_3D('',#5747,#4707,#4708);
#4099=AXIS2_PLACEMENT_3D('',#5751,#4710,#4711);
#4100=AXIS2_PLACEMENT_3D('',#5755,#4713,#4714);
#4101=AXIS2_PLACEMENT_3D('',#5759,#4716,#4717);
#4102=AXIS2_PLACEMENT_3D('',#5763,#4719,#4720);
#4103=AXIS2_PLACEMENT_3D('',#5765,#4722,#4723);
#4104=AXIS2_PLACEMENT_3D('',#5769,#4726,#4727);
#4105=AXIS2_PLACEMENT_3D('',#5771,#4728,#4729);
#4106=AXIS2_PLACEMENT_3D('',#5773,#4731,#4732);
#4107=AXIS2_PLACEMENT_3D('',#5777,#4734,#4735);
#4108=AXIS2_PLACEMENT_3D('',#5779,#4737,#4738);
#4109=AXIS2_PLACEMENT_3D('',#5783,#4741,#4742);
#4110=AXIS2_PLACEMENT_3D('',#5785,#4743,#4744);
#4111=AXIS2_PLACEMENT_3D('',#5787,#4746,#4747);
#4112=AXIS2_PLACEMENT_3D('',#5790,#4748,#4749);
#4113=AXIS2_PLACEMENT_3D('',#5793,#4752,#4753);
#4114=AXIS2_PLACEMENT_3D('',#5797,#4756,#4757);
#4115=AXIS2_PLACEMENT_3D('',#5799,#4758,#4759);
#4116=AXIS2_PLACEMENT_3D('',#5801,#4761,#4762);
#4117=AXIS2_PLACEMENT_3D('',#5805,#4765,#4766);
#4118=AXIS2_PLACEMENT_3D('',#5807,#4767,#4768);
#4119=AXIS2_PLACEMENT_3D('',#5809,#4770,#4771);
#4120=AXIS2_PLACEMENT_3D('',#5813,#4773,#4774);
#4121=AXIS2_PLACEMENT_3D('',#5815,#4776,#4777);
#4122=AXIS2_PLACEMENT_3D('',#5817,#4779,#4780);
#4123=AXIS2_PLACEMENT_3D('',#5819,#4782,#4783);
#4124=AXIS2_PLACEMENT_3D('',#5821,#4785,#4786);
#4125=AXIS2_PLACEMENT_3D('',#5823,#4788,#4789);
#4126=AXIS2_PLACEMENT_3D('',#5824,#4790,#4791);
#4127=AXIS2_PLACEMENT_3D('',#5825,#4792,#4793);
#4128=AXIS2_PLACEMENT_3D('',#5827,#4794,#4795);
#4129=AXIS2_PLACEMENT_3D('',#5830,#4797,#4798);
#4130=AXIS2_PLACEMENT_3D('',#5831,#4799,#4800);
#4131=AXIS2_PLACEMENT_3D('',#5833,#4801,#4802);
#4132=AXIS2_PLACEMENT_3D('',#5836,#4804,#4805);
#4133=AXIS2_PLACEMENT_3D('',#5837,#4806,#4807);
#4134=AXIS2_PLACEMENT_3D('',#5839,#4808,#4809);
#4135=AXIS2_PLACEMENT_3D('',#5842,#4811,#4812);
#4136=AXIS2_PLACEMENT_3D('',#5843,#4813,#4814);
#4137=AXIS2_PLACEMENT_3D('',#5845,#4815,#4816);
#4138=AXIS2_PLACEMENT_3D('',#5848,#4818,#4819);
#4139=AXIS2_PLACEMENT_3D('',#5849,#4820,#4821);
#4140=AXIS2_PLACEMENT_3D('',#5851,#4822,#4823);
#4141=AXIS2_PLACEMENT_3D('',#5854,#4825,#4826);
#4142=AXIS2_PLACEMENT_3D('',#5855,#4827,#4828);
#4143=AXIS2_PLACEMENT_3D('',#5857,#4829,#4830);
#4144=AXIS2_PLACEMENT_3D('',#5860,#4832,#4833);
#4145=AXIS2_PLACEMENT_3D('',#5861,#4834,#4835);
#4146=AXIS2_PLACEMENT_3D('',#5863,#4836,#4837);
#4147=AXIS2_PLACEMENT_3D('',#5866,#4839,#4840);
#4148=AXIS2_PLACEMENT_3D('',#5867,#4841,#4842);
#4149=AXIS2_PLACEMENT_3D('',#5869,#4843,#4844);
#4150=AXIS2_PLACEMENT_3D('',#5872,#4846,#4847);
#4151=AXIS2_PLACEMENT_3D('',#5873,#4848,#4849);
#4152=AXIS2_PLACEMENT_3D('',#5882,#4854,#4855);
#4153=AXIS2_PLACEMENT_3D('',#5888,#4859,#4860);
#4154=AXIS2_PLACEMENT_3D('',#5897,#4865,#4866);
#4155=AXIS2_PLACEMENT_3D('',#5903,#4870,#4871);
#4156=AXIS2_PLACEMENT_3D('',#5912,#4876,#4877);
#4157=AXIS2_PLACEMENT_3D('',#5918,#4881,#4882);
#4158=AXIS2_PLACEMENT_3D('',#5927,#4887,#4888);
#4159=AXIS2_PLACEMENT_3D('',#5933,#4892,#4893);
#4160=AXIS2_PLACEMENT_3D('',#5936,#4896,#4897);
#4161=AXIS2_PLACEMENT_3D('',#5939,#4900,#4901);
#4162=AXIS2_PLACEMENT_3D('',#5942,#4904,#4905);
#4163=AXIS2_PLACEMENT_3D('',#5945,#4908,#4909);
#4164=AXIS2_PLACEMENT_3D('',#5946,#4910,#4911);
#4165=AXIS2_PLACEMENT_3D('',#5947,#4912,#4913);
#4166=AXIS2_PLACEMENT_3D('',#5948,#4914,#4915);
#4167=AXIS2_PLACEMENT_3D('',#5950,#4916,#4917);
#4168=AXIS2_PLACEMENT_3D('',#5953,#4919,#4920);
#4169=AXIS2_PLACEMENT_3D('',#5954,#4921,#4922);
#4170=AXIS2_PLACEMENT_3D('',#5956,#4923,#4924);
#4171=AXIS2_PLACEMENT_3D('',#5959,#4926,#4927);
#4172=AXIS2_PLACEMENT_3D('',#5960,#4928,#4929);
#4173=AXIS2_PLACEMENT_3D('',#5962,#4930,#4931);
#4174=AXIS2_PLACEMENT_3D('',#5965,#4933,#4934);
#4175=AXIS2_PLACEMENT_3D('',#5966,#4935,#4936);
#4176=AXIS2_PLACEMENT_3D('',#5968,#4937,#4938);
#4177=AXIS2_PLACEMENT_3D('',#5971,#4940,#4941);
#4178=AXIS2_PLACEMENT_3D('',#5972,#4942,#4943);
#4179=AXIS2_PLACEMENT_3D('',#5981,#4948,#4949);
#4180=AXIS2_PLACEMENT_3D('',#5987,#4953,#4954);
#4181=AXIS2_PLACEMENT_3D('',#5993,#4958,#4959);
#4182=AXIS2_PLACEMENT_3D('',#5996,#4962,#4963);
#4183=AXIS2_PLACEMENT_3D('',#5997,#4964,#4965);
#4184=AXIS2_PLACEMENT_3D('',#5998,#4966,#4967);
#4185=AXIS2_PLACEMENT_3D('',#5999,#4968,#4969);
#4186=AXIS2_PLACEMENT_3D('',#6001,#4970,#4971);
#4187=AXIS2_PLACEMENT_3D('',#6004,#4973,#4974);
#4188=AXIS2_PLACEMENT_3D('',#6005,#4975,#4976);
#4189=AXIS2_PLACEMENT_3D('',#6007,#4977,#4978);
#4190=AXIS2_PLACEMENT_3D('',#6010,#4980,#4981);
#4191=AXIS2_PLACEMENT_3D('',#6011,#4982,#4983);
#4192=AXIS2_PLACEMENT_3D('',#6013,#4984,#4985);
#4193=AXIS2_PLACEMENT_3D('',#6016,#4987,#4988);
#4194=AXIS2_PLACEMENT_3D('',#6017,#4989,#4990);
#4195=AXIS2_PLACEMENT_3D('',#6019,#4991,#4992);
#4196=AXIS2_PLACEMENT_3D('',#6022,#4994,#4995);
#4197=AXIS2_PLACEMENT_3D('',#6023,#4996,#4997);
#4198=AXIS2_PLACEMENT_3D('',#6032,#5002,#5003);
#4199=AXIS2_PLACEMENT_3D('',#6038,#5007,#5008);
#4200=AXIS2_PLACEMENT_3D('',#6044,#5012,#5013);
#4201=AXIS2_PLACEMENT_3D('',#6047,#5016,#5017);
#4202=AXIS2_PLACEMENT_3D('',#6048,#5018,#5019);
#4203=AXIS2_PLACEMENT_3D('',#6049,#5020,#5021);
#4204=AXIS2_PLACEMENT_3D('',#6050,#5022,#5023);
#4205=AXIS2_PLACEMENT_3D('',#6059,#5028,#5029);
#4206=AXIS2_PLACEMENT_3D('',#6065,#5033,#5034);
#4207=AXIS2_PLACEMENT_3D('',#6071,#5038,#5039);
#4208=AXIS2_PLACEMENT_3D('',#6074,#5042,#5043);
#4209=AXIS2_PLACEMENT_3D('',#6075,#5044,#5045);
#4210=AXIS2_PLACEMENT_3D('',#6076,#5046,#5047);
#4211=AXIS2_PLACEMENT_3D('',#6077,#5048,#5049);
#4212=AXIS2_PLACEMENT_3D('',#6086,#5054,#5055);
#4213=AXIS2_PLACEMENT_3D('',#6092,#5059,#5060);
#4214=AXIS2_PLACEMENT_3D('',#6095,#5063,#5064);
#4215=AXIS2_PLACEMENT_3D('',#6096,#5065,#5066);
#4216=AXIS2_PLACEMENT_3D('',#6097,#5067,#5068);
#4217=AXIS2_PLACEMENT_3D('',#6098,#5069,#5070);
#4218=AXIS2_PLACEMENT_3D('',#6117,#5072,#5073);
#4219=AXIS2_PLACEMENT_3D('',#6137,#5074,#5075);
#4220=AXIS2_PLACEMENT_3D('',#6188,#5077,#5078);
#4221=AXIS2_PLACEMENT_3D('',#6239,#5080,#5081);
#4222=AXIS2_PLACEMENT_3D('',#6287,#5083,#5084);
#4223=AXIS2_PLACEMENT_3D('',#6338,#5086,#5087);
#4224=AXIS2_PLACEMENT_3D('',#6389,#5089,#5090);
#4225=AXIS2_PLACEMENT_3D('',#6437,#5092,#5093);
#4226=AXIS2_PLACEMENT_3D('',#6488,#5095,#5096);
#4227=AXIS2_PLACEMENT_3D('',#6498,#5098,#5099);
#4228=AXIS2_PLACEMENT_3D('',#6509,#5100,#5101);
#4229=AXIS2_PLACEMENT_3D('',#6523,#5103,#5104);
#4230=AXIS2_PLACEMENT_3D('',#6533,#5105,#5106);
#4231=AXIS2_PLACEMENT_3D('',#6557,#5108,#5109);
#4232=AXIS2_PLACEMENT_3D('',#6582,#5111,#5112);
#4233=AXIS2_PLACEMENT_3D('',#6607,#5114,#5115);
#4234=AXIS2_PLACEMENT_3D('',#6631,#5117,#5118);
#4235=AXIS2_PLACEMENT_3D('',#6656,#5120,#5121);
#4236=AXIS2_PLACEMENT_3D('',#6681,#5123,#5124);
#4237=AXIS2_PLACEMENT_3D('',#6705,#5126,#5127);
#4238=AXIS2_PLACEMENT_3D('',#6716,#5129,#5130);
#4239=AXIS2_PLACEMENT_3D('',#6722,#5131,#5132);
#4240=AXIS2_PLACEMENT_3D('',#7651,#5133,#5134);
#4241=AXIS2_PLACEMENT_3D('',#7653,#5135,#5136);
#4242=AXIS2_PLACEMENT_3D('',#7654,#5137,#5138);
#4243=AXIS2_PLACEMENT_3D('',#7656,#5139,#5140);
#4244=AXIS2_PLACEMENT_3D('',#7658,#5141,#5142);
#4245=AXIS2_PLACEMENT_3D('',#7659,#5143,#5144);
#4246=AXIS2_PLACEMENT_3D('',#7661,#5145,#5146);
#4247=AXIS2_PLACEMENT_3D('',#7663,#5147,#5148);
#4248=AXIS2_PLACEMENT_3D('',#7664,#5149,#5150);
#4249=AXIS2_PLACEMENT_3D('',#7666,#5152,#5153);
#4250=AXIS2_PLACEMENT_3D('',#7669,#5155,#5156);
#4251=AXIS2_PLACEMENT_3D('',#7670,#5157,#5158);
#4252=AXIS2_PLACEMENT_3D('',#7672,#5159,#5160);
#4253=AXIS2_PLACEMENT_3D('',#7674,#5161,#5162);
#4254=AXIS2_PLACEMENT_3D('',#7675,#5163,#5164);
#4255=AXIS2_PLACEMENT_3D('',#7677,#5166,#5167);
#4256=AXIS2_PLACEMENT_3D('',#7678,#5168,#5169);
#4257=AXIS2_PLACEMENT_3D('',#7680,#5171,#5172);
#4258=AXIS2_PLACEMENT_3D('',#7681,#5173,#5174);
#4259=AXIS2_PLACEMENT_3D('',#7682,#5175,#5176);
#4260=AXIS2_PLACEMENT_3D('',#7698,#5178,#5179);
#4261=AXIS2_PLACEMENT_3D('',#7706,#5180,#5181);
#4262=AXIS2_PLACEMENT_3D('',#7754,#5183,#5184);
#4263=AXIS2_PLACEMENT_3D('',#7802,#5186,#5187);
#4264=AXIS2_PLACEMENT_3D('',#7856,#5189,#5190);
#4265=AXIS2_PLACEMENT_3D('',#7904,#5192,#5193);
#4266=AXIS2_PLACEMENT_3D('',#7952,#5195,#5196);
#4267=AXIS2_PLACEMENT_3D('',#8006,#5198,#5199);
#4268=AXIS2_PLACEMENT_3D('',#8054,#5201,#5202);
#4269=AXIS2_PLACEMENT_3D('',#8105,#5204,#5205);
#4270=AXIS2_PLACEMENT_3D('',#8156,#5207,#5208);
#4271=AXIS2_PLACEMENT_3D('',#8204,#5210,#5211);
#4272=AXIS2_PLACEMENT_3D('',#8220,#5213,#5214);
#4273=AXIS2_PLACEMENT_3D('',#8229,#5215,#5216);
#4274=AXIS2_PLACEMENT_3D('',#8254,#5218,#5219);
#4275=AXIS2_PLACEMENT_3D('',#8278,#5221,#5222);
#4276=AXIS2_PLACEMENT_3D('',#8304,#5224,#5225);
#4277=AXIS2_PLACEMENT_3D('',#8328,#5227,#5228);
#4278=AXIS2_PLACEMENT_3D('',#8353,#5230,#5231);
#4279=AXIS2_PLACEMENT_3D('',#8378,#5233,#5234);
#4280=AXIS2_PLACEMENT_3D('',#8402,#5236,#5237);
#4281=AXIS2_PLACEMENT_3D('',#8427,#5239,#5240);
#4282=AXIS2_PLACEMENT_3D('',#8452,#5242,#5243);
#4283=AXIS2_PLACEMENT_3D('',#8476,#5245,#5246);
#4284=AXIS2_PLACEMENT_3D('',#8758,#5247,#5248);
#4285=AXIS2_PLACEMENT_3D('',#8792,#5250,#5251);
#4286=AXIS2_PLACEMENT_3D('',#9217,#5252,#5253);
#4287=AXIS2_PLACEMENT_3D('',#9228,#5254,#5255);
#4288=AXIS2_PLACEMENT_3D('',#9655,#5256,#5257);
#4289=AXIS2_PLACEMENT_3D('',#9656,#5258,#5259);
#4290=AXIS2_PLACEMENT_3D('',#9665,#5264,#5265);
#4291=AXIS2_PLACEMENT_3D('',#9671,#5269,#5270);
#4292=AXIS2_PLACEMENT_3D('',#9677,#5274,#5275);
#4293=AXIS2_PLACEMENT_3D('',#9683,#5279,#5280);
#4294=AXIS2_PLACEMENT_3D('',#9689,#5284,#5285);
#4295=AXIS2_PLACEMENT_3D('',#9692,#5288,#5289);
#4296=AXIS2_PLACEMENT_3D('',#9693,#5290,#5291);
#4297=AXIS2_PLACEMENT_3D('',#9695,#5292,#5293);
#4298=AXIS2_PLACEMENT_3D('',#9696,#5294,#5295);
#4299=AXIS2_PLACEMENT_3D('',#9699,#5297,#5298);
#4300=AXIS2_PLACEMENT_3D('',#9700,#5299,#5300);
#4301=AXIS2_PLACEMENT_3D('',#9701,#5301,#5302);
#4302=AXIS2_PLACEMENT_3D('',#9702,#5303,#5304);
#4303=AXIS2_PLACEMENT_3D('',#9703,#5305,#5306);
#4304=AXIS2_PLACEMENT_3D('',#9704,#5307,#5308);
#4305=AXIS2_PLACEMENT_3D('',#9705,#5309,#5310);
#4306=AXIS2_PLACEMENT_3D('',#9706,#5311,#5312);
#4307=AXIS2_PLACEMENT_3D('',#9707,#5313,#5314);
#4308=AXIS2_PLACEMENT_3D('',#9708,#5315,#5316);
#4309=AXIS2_PLACEMENT_3D('',#9709,#5317,#5318);
#4310=AXIS2_PLACEMENT_3D('',#9710,#5319,#5320);
#4311=AXIS2_PLACEMENT_3D('',#9711,#5321,#5322);
#4312=AXIS2_PLACEMENT_3D('',#9712,#5323,#5324);
#4313=AXIS2_PLACEMENT_3D('',#9713,#5325,#5326);
#4314=AXIS2_PLACEMENT_3D('',#9714,#5327,#5328);
#4315=AXIS2_PLACEMENT_3D('',#9715,#5329,#5330);
#4316=AXIS2_PLACEMENT_3D('',#9716,#5331,#5332);
#4317=AXIS2_PLACEMENT_3D('',#9717,#5333,#5334);
#4318=AXIS2_PLACEMENT_3D('',#9718,#5335,#5336);
#4319=AXIS2_PLACEMENT_3D('',#9719,#5337,#5338);
#4320=AXIS2_PLACEMENT_3D('',#9720,#5339,#5340);
#4321=AXIS2_PLACEMENT_3D('',#9721,#5341,#5342);
#4322=AXIS2_PLACEMENT_3D('',#9722,#5343,#5344);
#4323=AXIS2_PLACEMENT_3D('',#9723,#5345,#5346);
#4324=AXIS2_PLACEMENT_3D('',#9724,#5347,#5348);
#4325=AXIS2_PLACEMENT_3D('',#9725,#5349,#5350);
#4326=AXIS2_PLACEMENT_3D('',#9726,#5351,#5352);
#4327=AXIS2_PLACEMENT_3D('',#9727,#5353,#5354);
#4328=AXIS2_PLACEMENT_3D('',#9728,#5355,#5356);
#4329=AXIS2_PLACEMENT_3D('',#9729,#5357,#5358);
#4330=AXIS2_PLACEMENT_3D('',#9730,#5359,#5360);
#4331=AXIS2_PLACEMENT_3D('',#9731,#5361,#5362);
#4332=AXIS2_PLACEMENT_3D('',#9732,#5363,#5364);
#4333=AXIS2_PLACEMENT_3D('',#9733,#5365,#5366);
#4334=AXIS2_PLACEMENT_3D('',#9734,#5367,#5368);
#4335=AXIS2_PLACEMENT_3D('',#9735,#5369,#5370);
#4336=AXIS2_PLACEMENT_3D('',#9736,#5371,#5372);
#4337=AXIS2_PLACEMENT_3D('',#9737,#5373,#5374);
#4338=AXIS2_PLACEMENT_3D('',#9738,#5375,#5376);
#4339=AXIS2_PLACEMENT_3D('',#9739,#5377,#5378);
#4340=AXIS2_PLACEMENT_3D('',#9740,#5379,#5380);
#4341=AXIS2_PLACEMENT_3D('',#9741,#5381,#5382);
#4342=AXIS2_PLACEMENT_3D('',#9742,#5383,#5384);
#4343=AXIS2_PLACEMENT_3D('',#9743,#5385,#5386);
#4344=AXIS2_PLACEMENT_3D('',#9744,#5387,#5388);
#4345=AXIS2_PLACEMENT_3D('',#9745,#5389,#5390);
#4346=AXIS2_PLACEMENT_3D('',#9746,#5391,#5392);
#4347=AXIS2_PLACEMENT_3D('',#9747,#5393,#5394);
#4348=AXIS2_PLACEMENT_3D('',#9748,#5395,#5396);
#4349=AXIS2_PLACEMENT_3D('',#9749,#5397,#5398);
#4350=AXIS2_PLACEMENT_3D('',#9750,#5399,#5400);
#4351=AXIS2_PLACEMENT_3D('',#9751,#5401,#5402);
#4352=DIRECTION('axis',(0.,0.,1.));
#4353=DIRECTION('refdir',(1.,0.,0.));
#4354=DIRECTION('axis',(0.,0.,1.));
#4355=DIRECTION('refdir',(1.,0.,0.));
#4356=DIRECTION('center_axis',(0.,0.,1.));
#4357=DIRECTION('ref_axis',(-0.707106781186548,-0.707106781186548,0.));
#4358=DIRECTION('center_axis',(0.,0.,-1.));
#4359=DIRECTION('ref_axis',(-0.707106781186548,-0.707106781186548,0.));
#4360=DIRECTION('',(0.,0.,-1.));
#4361=DIRECTION('center_axis',(0.,0.,1.));
#4362=DIRECTION('ref_axis',(-0.707106781186548,-0.707106781186548,0.));
#4363=DIRECTION('',(0.,0.,1.));
#4364=DIRECTION('center_axis',(-1.,0.,0.));
#4365=DIRECTION('ref_axis',(0.,-1.,0.));
#4366=DIRECTION('',(0.,-1.,0.));
#4367=DIRECTION('',(0.,0.,1.));
#4368=DIRECTION('',(0.,-1.,0.));
#4369=DIRECTION('center_axis',(0.,0.,1.));
#4370=DIRECTION('ref_axis',(1.,0.,0.));
#4371=DIRECTION('',(1.,0.,0.));
#4372=DIRECTION('center_axis',(0.,0.,-1.));
#4373=DIRECTION('ref_axis',(0.707106781186548,-0.707106781186548,0.));
#4374=DIRECTION('',(0.,1.,0.));
#4375=DIRECTION('center_axis',(0.,0.,-1.));
#4376=DIRECTION('ref_axis',(0.707106781186548,0.707106781186548,0.));
#4377=DIRECTION('',(-1.,0.,0.));
#4378=DIRECTION('center_axis',(0.,0.,-1.));
#4379=DIRECTION('ref_axis',(-0.707106781186548,0.707106781186548,0.));
#4380=DIRECTION('',(0.,1.,0.));
#4381=DIRECTION('center_axis',(0.,0.,1.));
#4382=DIRECTION('ref_axis',(-0.707106781186548,0.707106781186548,0.));
#4383=DIRECTION('',(1.,0.,0.));
#4384=DIRECTION('center_axis',(0.,0.,1.));
#4385=DIRECTION('ref_axis',(0.707106781186548,0.707106781186548,0.));
#4386=DIRECTION('',(0.,-1.,0.));
#4387=DIRECTION('center_axis',(0.,0.,1.));
#4388=DIRECTION('ref_axis',(0.707106781186548,-0.707106781186548,0.));
#4389=DIRECTION('',(-1.,0.,0.));
#4390=DIRECTION('center_axis',(0.,0.,1.));
#4391=DIRECTION('ref_axis',(-0.707106781186548,-0.707106781186548,0.));
#4392=DIRECTION('center_axis',(0.,0.,1.));
#4393=DIRECTION('ref_axis',(0.707106781186548,-0.707106781186548,0.));
#4394=DIRECTION('',(0.,0.,-1.));
#4395=DIRECTION('center_axis',(0.,0.,1.));
#4396=DIRECTION('ref_axis',(0.707106781186548,-0.707106781186548,0.));
#4397=DIRECTION('',(0.,0.,1.));
#4398=DIRECTION('center_axis',(1.,0.,0.));
#4399=DIRECTION('ref_axis',(0.,1.,0.));
#4400=DIRECTION('',(0.,1.,0.));
#4401=DIRECTION('',(0.,0.,-1.));
#4402=DIRECTION('center_axis',(0.,0.,1.));
#4403=DIRECTION('ref_axis',(0.707106781186548,0.707106781186548,0.));
#4404=DIRECTION('center_axis',(0.,0.,1.));
#4405=DIRECTION('ref_axis',(0.707106781186548,0.707106781186548,0.));
#4406=DIRECTION('',(0.,0.,1.));
#4407=DIRECTION('center_axis',(0.,0.,1.));
#4408=DIRECTION('ref_axis',(-0.707106781186548,0.707106781186548,0.));
#4409=DIRECTION('',(0.,0.,-1.));
#4410=DIRECTION('center_axis',(0.,0.,1.));
#4411=DIRECTION('ref_axis',(-0.707106781186548,0.707106781186548,0.));
#4412=DIRECTION('center_axis',(0.,0.,1.));
#4413=DIRECTION('ref_axis',(-0.707106781186548,0.707106781186548,0.));
#4414=DIRECTION('center_axis',(0.,0.,-1.));
#4415=DIRECTION('ref_axis',(-0.707106781186548,0.707106781186548,0.));
#4416=DIRECTION('',(0.,0.,1.));
#4417=DIRECTION('',(0.,0.,-1.));
#4418=DIRECTION('center_axis',(0.,-1.,0.));
#4419=DIRECTION('ref_axis',(1.,0.,0.));
#4420=DIRECTION('',(1.,0.,0.));
#4421=DIRECTION('',(0.,0.,-1.));
#4422=DIRECTION('center_axis',(0.,0.,1.));
#4423=DIRECTION('ref_axis',(0.707106781186548,0.707106781186548,0.));
#4424=DIRECTION('center_axis',(0.,0.,-1.));
#4425=DIRECTION('ref_axis',(0.707106781186548,0.707106781186548,0.));
#4426=DIRECTION('',(0.,0.,1.));
#4427=DIRECTION('center_axis',(-1.,0.,0.));
#4428=DIRECTION('ref_axis',(0.,-1.,0.));
#4429=DIRECTION('',(0.,-1.,0.));
#4430=DIRECTION('',(0.,0.,-1.));
#4431=DIRECTION('center_axis',(0.,0.,1.));
#4432=DIRECTION('ref_axis',(0.707106781186548,-0.707106781186548,0.));
#4433=DIRECTION('center_axis',(0.,0.,-1.));
#4434=DIRECTION('ref_axis',(0.707106781186548,-0.707106781186548,0.));
#4435=DIRECTION('',(0.,0.,1.));
#4436=DIRECTION('center_axis',(0.,1.,0.));
#4437=DIRECTION('ref_axis',(-1.,0.,0.));
#4438=DIRECTION('',(-1.,0.,0.));
#4439=DIRECTION('',(0.,0.,-1.));
#4440=DIRECTION('center_axis',(0.,0.,1.));
#4441=DIRECTION('ref_axis',(-0.707106781186548,-0.707106781186548,0.));
#4442=DIRECTION('center_axis',(0.,0.,-1.));
#4443=DIRECTION('ref_axis',(-0.707106781186548,-0.707106781186548,0.));
#4444=DIRECTION('',(0.,0.,1.));
#4445=DIRECTION('center_axis',(1.,0.,0.));
#4446=DIRECTION('ref_axis',(0.,1.,0.));
#4447=DIRECTION('',(0.,1.,0.));
#4448=DIRECTION('center_axis',(0.,1.,0.));
#4449=DIRECTION('ref_axis',(-1.,0.,0.));
#4450=DIRECTION('',(-1.,0.,0.));
#4451=DIRECTION('center_axis',(0.,-1.,0.));
#4452=DIRECTION('ref_axis',(1.,0.,0.));
#4453=DIRECTION('',(1.,0.,0.));
#4454=DIRECTION('center_axis',(0.,0.,1.));
#4455=DIRECTION('ref_axis',(1.,0.,0.));
#4456=DIRECTION('axis',(0.,0.,1.));
#4457=DIRECTION('refdir',(1.,0.,0.));
#4458=DIRECTION('center_axis',(0.,-1.,0.));
#4459=DIRECTION('ref_axis',(0.,0.,1.));
#4460=DIRECTION('center_axis',(0.,-1.,0.));
#4461=DIRECTION('ref_axis',(0.,0.,1.));
#4462=DIRECTION('',(0.,-1.,0.));
#4463=DIRECTION('center_axis',(0.,1.,0.));
#4464=DIRECTION('ref_axis',(0.,0.,1.));
#4465=DIRECTION('center_axis',(0.,-1.,0.));
#4466=DIRECTION('ref_axis',(0.,0.,1.));
#4467=DIRECTION('center_axis',(0.,-1.,0.));
#4468=DIRECTION('ref_axis',(0.,0.,1.));
#4469=DIRECTION('',(0.,-1.,0.));
#4470=DIRECTION('center_axis',(0.,1.,0.));
#4471=DIRECTION('ref_axis',(0.,0.,1.));
#4472=DIRECTION('center_axis',(0.,0.,1.));
#4473=DIRECTION('ref_axis',(-0.707106781186548,-0.707106781186548,0.));
#4474=DIRECTION('center_axis',(0.,0.,-1.));
#4475=DIRECTION('ref_axis',(-0.707106781186548,-0.707106781186548,0.));
#4476=DIRECTION('',(0.,0.,-1.));
#4477=DIRECTION('center_axis',(0.,0.,1.));
#4478=DIRECTION('ref_axis',(-0.707106781186548,-0.707106781186548,0.));
#4479=DIRECTION('',(0.,0.,1.));
#4480=DIRECTION('center_axis',(-1.,0.,0.));
#4481=DIRECTION('ref_axis',(0.,-1.,0.));
#4482=DIRECTION('',(0.,-1.,0.));
#4483=DIRECTION('',(0.,0.,1.));
#4484=DIRECTION('',(0.,-1.,0.));
#4485=DIRECTION('center_axis',(0.,0.,1.));
#4486=DIRECTION('ref_axis',(1.,0.,0.));
#4487=DIRECTION('',(1.,0.,0.));
#4488=DIRECTION('center_axis',(0.,0.,-1.));
#4489=DIRECTION('ref_axis',(0.707106781186548,-0.707106781186548,0.));
#4490=DIRECTION('',(0.,1.,0.));
#4491=DIRECTION('center_axis',(0.,0.,-1.));
#4492=DIRECTION('ref_axis',(0.707106781186548,0.707106781186548,0.));
#4493=DIRECTION('',(-1.,0.,0.));
#4494=DIRECTION('center_axis',(0.,0.,-1.));
#4495=DIRECTION('ref_axis',(-0.707106781186548,0.707106781186548,0.));
#4496=DIRECTION('',(0.,1.,0.));
#4497=DIRECTION('center_axis',(0.,0.,1.));
#4498=DIRECTION('ref_axis',(-0.707106781186548,0.707106781186548,0.));
#4499=DIRECTION('',(1.,0.,0.));
#4500=DIRECTION('center_axis',(0.,0.,1.));
#4501=DIRECTION('ref_axis',(0.707106781186548,0.707106781186548,0.));
#4502=DIRECTION('',(0.,-1.,0.));
#4503=DIRECTION('center_axis',(0.,0.,1.));
#4504=DIRECTION('ref_axis',(0.707106781186548,-0.707106781186548,0.));
#4505=DIRECTION('',(-1.,0.,0.));
#4506=DIRECTION('center_axis',(0.,0.,1.));
#4507=DIRECTION('ref_axis',(-0.707106781186548,-0.707106781186548,0.));
#4508=DIRECTION('center_axis',(0.,0.,1.));
#4509=DIRECTION('ref_axis',(0.707106781186548,-0.707106781186548,0.));
#4510=DIRECTION('',(0.,0.,-1.));
#4511=DIRECTION('center_axis',(0.,0.,1.));
#4512=DIRECTION('ref_axis',(0.707106781186548,-0.707106781186548,0.));
#4513=DIRECTION('',(0.,0.,1.));
#4514=DIRECTION('center_axis',(1.,0.,0.));
#4515=DIRECTION('ref_axis',(0.,1.,0.));
#4516=DIRECTION('',(0.,1.,0.));
#4517=DIRECTION('',(0.,0.,-1.));
#4518=DIRECTION('center_axis',(0.,0.,1.));
#4519=DIRECTION('ref_axis',(0.707106781186548,0.707106781186548,0.));
#4520=DIRECTION('center_axis',(0.,0.,1.));
#4521=DIRECTION('ref_axis',(0.707106781186548,0.707106781186548,0.));
#4522=DIRECTION('',(0.,0.,1.));
#4523=DIRECTION('center_axis',(0.,0.,1.));
#4524=DIRECTION('ref_axis',(-0.707106781186548,0.707106781186548,0.));
#4525=DIRECTION('',(0.,0.,-1.));
#4526=DIRECTION('center_axis',(0.,0.,1.));
#4527=DIRECTION('ref_axis',(-0.707106781186548,0.707106781186548,0.));
#4528=DIRECTION('center_axis',(0.,0.,1.));
#4529=DIRECTION('ref_axis',(-0.707106781186548,0.707106781186548,0.));
#4530=DIRECTION('center_axis',(0.,0.,-1.));
#4531=DIRECTION('ref_axis',(-0.707106781186548,0.707106781186548,0.));
#4532=DIRECTION('',(0.,0.,1.));
#4533=DIRECTION('',(0.,0.,-1.));
#4534=DIRECTION('center_axis',(0.,-1.,0.));
#4535=DIRECTION('ref_axis',(1.,0.,0.));
#4536=DIRECTION('',(1.,0.,0.));
#4537=DIRECTION('',(0.,0.,-1.));
#4538=DIRECTION('center_axis',(0.,0.,1.));
#4539=DIRECTION('ref_axis',(0.707106781186548,0.707106781186548,0.));
#4540=DIRECTION('center_axis',(0.,0.,-1.));
#4541=DIRECTION('ref_axis',(0.707106781186548,0.707106781186548,0.));
#4542=DIRECTION('',(0.,0.,1.));
#4543=DIRECTION('center_axis',(-1.,0.,0.));
#4544=DIRECTION('ref_axis',(0.,-1.,0.));
#4545=DIRECTION('',(0.,-1.,0.));
#4546=DIRECTION('',(0.,0.,-1.));
#4547=DIRECTION('center_axis',(0.,0.,1.));
#4548=DIRECTION('ref_axis',(0.707106781186548,-0.707106781186548,0.));
#4549=DIRECTION('center_axis',(0.,0.,-1.));
#4550=DIRECTION('ref_axis',(0.707106781186548,-0.707106781186548,0.));
#4551=DIRECTION('',(0.,0.,1.));
#4552=DIRECTION('center_axis',(0.,1.,0.));
#4553=DIRECTION('ref_axis',(-1.,0.,0.));
#4554=DIRECTION('',(-1.,0.,0.));
#4555=DIRECTION('',(0.,0.,-1.));
#4556=DIRECTION('center_axis',(0.,0.,1.));
#4557=DIRECTION('ref_axis',(-0.707106781186548,-0.707106781186548,0.));
#4558=DIRECTION('center_axis',(0.,0.,-1.));
#4559=DIRECTION('ref_axis',(-0.707106781186548,-0.707106781186548,0.));
#4560=DIRECTION('',(0.,0.,1.));
#4561=DIRECTION('center_axis',(1.,0.,0.));
#4562=DIRECTION('ref_axis',(0.,1.,0.));
#4563=DIRECTION('',(0.,1.,0.));
#4564=DIRECTION('center_axis',(0.,1.,0.));
#4565=DIRECTION('ref_axis',(-1.,0.,0.));
#4566=DIRECTION('',(-1.,0.,0.));
#4567=DIRECTION('center_axis',(0.,-1.,0.));
#4568=DIRECTION('ref_axis',(1.,0.,0.));
#4569=DIRECTION('',(1.,0.,0.));
#4570=DIRECTION('center_axis',(0.,0.,1.));
#4571=DIRECTION('ref_axis',(1.,0.,0.));
#4572=DIRECTION('axis',(0.,0.,1.));
#4573=DIRECTION('refdir',(1.,0.,0.));
#4574=DIRECTION('center_axis',(0.,0.,1.));
#4575=DIRECTION('ref_axis',(-0.707106781186548,-0.707106781186548,0.));
#4576=DIRECTION('center_axis',(0.,0.,-1.));
#4577=DIRECTION('ref_axis',(-0.707106781186548,-0.707106781186548,0.));
#4578=DIRECTION('',(0.,0.,-1.));
#4579=DIRECTION('center_axis',(0.,0.,1.));
#4580=DIRECTION('ref_axis',(-0.707106781186548,-0.707106781186548,0.));
#4581=DIRECTION('',(0.,0.,1.));
#4582=DIRECTION('center_axis',(-1.,0.,0.));
#4583=DIRECTION('ref_axis',(0.,-1.,0.));
#4584=DIRECTION('',(0.,-1.,0.));
#4585=DIRECTION('',(0.,0.,1.));
#4586=DIRECTION('',(0.,-1.,0.));
#4587=DIRECTION('center_axis',(0.,0.,1.));
#4588=DIRECTION('ref_axis',(1.,0.,0.));
#4589=DIRECTION('',(1.,0.,0.));
#4590=DIRECTION('center_axis',(0.,0.,-1.));
#4591=DIRECTION('ref_axis',(0.707106781186548,-0.707106781186548,0.));
#4592=DIRECTION('',(0.,1.,0.));
#4593=DIRECTION('center_axis',(0.,0.,-1.));
#4594=DIRECTION('ref_axis',(0.707106781186548,0.707106781186548,0.));
#4595=DIRECTION('',(-1.,0.,0.));
#4596=DIRECTION('center_axis',(0.,0.,-1.));
#4597=DIRECTION('ref_axis',(-0.707106781186548,0.707106781186548,0.));
#4598=DIRECTION('',(0.,1.,0.));
#4599=DIRECTION('center_axis',(0.,0.,1.));
#4600=DIRECTION('ref_axis',(-0.707106781186548,0.707106781186548,0.));
#4601=DIRECTION('',(1.,0.,0.));
#4602=DIRECTION('center_axis',(0.,0.,1.));
#4603=DIRECTION('ref_axis',(0.707106781186548,0.707106781186548,0.));
#4604=DIRECTION('',(0.,-1.,0.));
#4605=DIRECTION('center_axis',(0.,0.,1.));
#4606=DIRECTION('ref_axis',(0.707106781186548,-0.707106781186548,0.));
#4607=DIRECTION('',(-1.,0.,0.));
#4608=DIRECTION('center_axis',(0.,0.,1.));
#4609=DIRECTION('ref_axis',(-0.707106781186548,-0.707106781186548,0.));
#4610=DIRECTION('center_axis',(0.,0.,1.));
#4611=DIRECTION('ref_axis',(0.707106781186548,-0.707106781186548,0.));
#4612=DIRECTION('',(0.,0.,-1.));
#4613=DIRECTION('center_axis',(0.,0.,1.));
#4614=DIRECTION('ref_axis',(0.707106781186548,-0.707106781186548,0.));
#4615=DIRECTION('',(0.,0.,1.));
#4616=DIRECTION('center_axis',(1.,0.,0.));
#4617=DIRECTION('ref_axis',(0.,1.,0.));
#4618=DIRECTION('',(0.,1.,0.));
#4619=DIRECTION('',(0.,0.,-1.));
#4620=DIRECTION('center_axis',(0.,0.,1.));
#4621=DIRECTION('ref_axis',(0.707106781186548,0.707106781186548,0.));
#4622=DIRECTION('center_axis',(0.,0.,1.));
#4623=DIRECTION('ref_axis',(0.707106781186548,0.707106781186548,0.));
#4624=DIRECTION('',(0.,0.,1.));
#4625=DIRECTION('center_axis',(0.,0.,1.));
#4626=DIRECTION('ref_axis',(-0.707106781186548,0.707106781186548,0.));
#4627=DIRECTION('',(0.,0.,-1.));
#4628=DIRECTION('center_axis',(0.,0.,1.));
#4629=DIRECTION('ref_axis',(-0.707106781186548,0.707106781186548,0.));
#4630=DIRECTION('center_axis',(0.,0.,1.));
#4631=DIRECTION('ref_axis',(-0.707106781186548,0.707106781186548,0.));
#4632=DIRECTION('center_axis',(0.,0.,-1.));
#4633=DIRECTION('ref_axis',(-0.707106781186548,0.707106781186548,0.));
#4634=DIRECTION('',(0.,0.,1.));
#4635=DIRECTION('',(0.,0.,-1.));
#4636=DIRECTION('center_axis',(0.,-1.,0.));
#4637=DIRECTION('ref_axis',(1.,0.,0.));
#4638=DIRECTION('',(1.,0.,0.));
#4639=DIRECTION('',(0.,0.,-1.));
#4640=DIRECTION('center_axis',(0.,0.,1.));
#4641=DIRECTION('ref_axis',(0.707106781186548,0.707106781186548,0.));
#4642=DIRECTION('center_axis',(0.,0.,-1.));
#4643=DIRECTION('ref_axis',(0.707106781186548,0.707106781186548,0.));
#4644=DIRECTION('',(0.,0.,1.));
#4645=DIRECTION('center_axis',(-1.,0.,0.));
#4646=DIRECTION('ref_axis',(0.,-1.,0.));
#4647=DIRECTION('',(0.,-1.,0.));
#4648=DIRECTION('',(0.,0.,-1.));
#4649=DIRECTION('center_axis',(0.,0.,1.));
#4650=DIRECTION('ref_axis',(0.707106781186548,-0.707106781186548,0.));
#4651=DIRECTION('center_axis',(0.,0.,-1.));
#4652=DIRECTION('ref_axis',(0.707106781186548,-0.707106781186548,0.));
#4653=DIRECTION('',(0.,0.,1.));
#4654=DIRECTION('center_axis',(0.,1.,0.));
#4655=DIRECTION('ref_axis',(-1.,0.,0.));
#4656=DIRECTION('',(-1.,0.,0.));
#4657=DIRECTION('',(0.,0.,-1.));
#4658=DIRECTION('center_axis',(0.,0.,1.));
#4659=DIRECTION('ref_axis',(-0.707106781186548,-0.707106781186548,0.));
#4660=DIRECTION('center_axis',(0.,0.,-1.));
#4661=DIRECTION('ref_axis',(-0.707106781186548,-0.707106781186548,0.));
#4662=DIRECTION('',(0.,0.,1.));
#4663=DIRECTION('center_axis',(1.,0.,0.));
#4664=DIRECTION('ref_axis',(0.,1.,0.));
#4665=DIRECTION('',(0.,1.,0.));
#4666=DIRECTION('center_axis',(0.,1.,0.));
#4667=DIRECTION('ref_axis',(-1.,0.,0.));
#4668=DIRECTION('',(-1.,0.,0.));
#4669=DIRECTION('center_axis',(0.,-1.,0.));
#4670=DIRECTION('ref_axis',(1.,0.,0.));
#4671=DIRECTION('',(1.,0.,0.));
#4672=DIRECTION('center_axis',(0.,0.,1.));
#4673=DIRECTION('ref_axis',(1.,0.,0.));
#4674=DIRECTION('axis',(0.,0.,1.));
#4675=DIRECTION('refdir',(1.,0.,0.));
#4676=DIRECTION('center_axis',(0.,-1.,0.));
#4677=DIRECTION('ref_axis',(0.,0.,1.));
#4678=DIRECTION('center_axis',(0.,-1.,0.));
#4679=DIRECTION('ref_axis',(0.,0.,1.));
#4680=DIRECTION('',(0.,-1.,0.));
#4681=DIRECTION('center_axis',(0.,1.,0.));
#4682=DIRECTION('ref_axis',(0.,0.,1.));
#4683=DIRECTION('center_axis',(0.,-1.,0.));
#4684=DIRECTION('ref_axis',(0.,0.,1.));
#4685=DIRECTION('center_axis',(0.,-1.,0.));
#4686=DIRECTION('ref_axis',(0.,0.,1.));
#4687=DIRECTION('',(0.,-1.,0.));
#4688=DIRECTION('center_axis',(0.,1.,0.));
#4689=DIRECTION('ref_axis',(0.,0.,1.));
#4690=DIRECTION('center_axis',(0.,0.,1.));
#4691=DIRECTION('ref_axis',(-0.707106781186547,-0.707106781186548,0.));
#4692=DIRECTION('center_axis',(0.,0.,-1.));
#4693=DIRECTION('ref_axis',(-0.707106781186547,-0.707106781186548,0.));
#4694=DIRECTION('',(0.,0.,-1.));
#4695=DIRECTION('center_axis',(0.,0.,1.));
#4696=DIRECTION('ref_axis',(-0.707106781186547,-0.707106781186548,0.));
#4697=DIRECTION('',(0.,0.,1.));
#4698=DIRECTION('center_axis',(0.,0.,1.));
#4699=DIRECTION('ref_axis',(1.,0.,0.));
#4700=DIRECTION('',(1.,0.,0.));
#4701=DIRECTION('center_axis',(0.,0.,-1.));
#4702=DIRECTION('ref_axis',(0.707106781186546,-0.707106781186549,0.));
#4703=DIRECTION('',(0.,1.,0.));
#4704=DIRECTION('center_axis',(0.,0.,-1.));
#4705=DIRECTION('ref_axis',(0.707106781186544,0.707106781186551,0.));
#4706=DIRECTION('',(-1.,0.,0.));
#4707=DIRECTION('center_axis',(0.,0.,-1.));
#4708=DIRECTION('ref_axis',(-0.707106781186548,0.707106781186548,0.));
#4709=DIRECTION('',(0.,-1.,0.));
#4710=DIRECTION('center_axis',(0.,0.,1.));
#4711=DIRECTION('ref_axis',(0.707106781186546,-0.707106781186549,0.));
#4712=DIRECTION('',(-1.,0.,0.));
#4713=DIRECTION('center_axis',(0.,0.,1.));
#4714=DIRECTION('ref_axis',(-0.707106781186546,-0.707106781186549,0.));
#4715=DIRECTION('',(0.,1.,0.));
#4716=DIRECTION('center_axis',(0.,0.,-1.));
#4717=DIRECTION('ref_axis',(0.707106781186546,0.707106781186549,0.));
#4718=DIRECTION('',(-1.,0.,0.));
#4719=DIRECTION('center_axis',(0.,0.,-1.));
#4720=DIRECTION('ref_axis',(-0.707106781186549,0.707106781186546,0.));
#4721=DIRECTION('',(0.,-1.,0.));
#4722=DIRECTION('center_axis',(0.,-1.,0.));
#4723=DIRECTION('ref_axis',(1.,0.,0.));
#4724=DIRECTION('',(1.,0.,0.));
#4725=DIRECTION('',(0.,0.,-1.));
#4726=DIRECTION('center_axis',(0.,0.,1.));
#4727=DIRECTION('ref_axis',(0.707106781186546,-0.707106781186549,0.));
#4728=DIRECTION('center_axis',(0.,0.,1.));
#4729=DIRECTION('ref_axis',(0.707106781186546,-0.707106781186549,0.));
#4730=DIRECTION('',(0.,0.,1.));
#4731=DIRECTION('center_axis',(0.,0.,1.));
#4732=DIRECTION('ref_axis',(0.707106781186544,0.707106781186551,0.));
#4733=DIRECTION('',(0.,0.,-1.));
#4734=DIRECTION('center_axis',(0.,0.,1.));
#4735=DIRECTION('ref_axis',(0.707106781186544,0.707106781186551,0.));
#4736=DIRECTION('',(0.,0.,1.));
#4737=DIRECTION('center_axis',(0.,1.,0.));
#4738=DIRECTION('ref_axis',(-1.,0.,0.));
#4739=DIRECTION('',(-1.,0.,0.));
#4740=DIRECTION('',(0.,0.,-1.));
#4741=DIRECTION('center_axis',(0.,0.,1.));
#4742=DIRECTION('ref_axis',(-0.707106781186548,0.707106781186548,0.));
#4743=DIRECTION('center_axis',(0.,0.,1.));
#4744=DIRECTION('ref_axis',(-0.707106781186548,0.707106781186548,0.));
#4745=DIRECTION('',(0.,0.,1.));
#4746=DIRECTION('center_axis',(0.,0.,1.));
#4747=DIRECTION('ref_axis',(0.707106781186546,-0.707106781186549,0.));
#4748=DIRECTION('center_axis',(0.,0.,-1.));
#4749=DIRECTION('ref_axis',(0.707106781186546,-0.707106781186549,0.));
#4750=DIRECTION('',(0.,0.,1.));
#4751=DIRECTION('',(0.,0.,-1.));
#4752=DIRECTION('center_axis',(0.,1.,0.));
#4753=DIRECTION('ref_axis',(-1.,0.,0.));
#4754=DIRECTION('',(-1.,0.,0.));
#4755=DIRECTION('',(0.,0.,-1.));
#4756=DIRECTION('center_axis',(0.,0.,1.));
#4757=DIRECTION('ref_axis',(-0.707106781186546,-0.707106781186549,0.));
#4758=DIRECTION('center_axis',(0.,0.,-1.));
#4759=DIRECTION('ref_axis',(-0.707106781186546,-0.707106781186549,0.));
#4760=DIRECTION('',(0.,0.,1.));
#4761=DIRECTION('center_axis',(1.,0.,0.));
#4762=DIRECTION('ref_axis',(0.,1.,0.));
#4763=DIRECTION('',(0.,1.,0.));
#4764=DIRECTION('',(0.,0.,-1.));
#4765=DIRECTION('center_axis',(0.,0.,1.));
#4766=DIRECTION('ref_axis',(0.707106781186546,0.707106781186549,0.));
#4767=DIRECTION('center_axis',(0.,0.,1.));
#4768=DIRECTION('ref_axis',(0.707106781186546,0.707106781186549,0.));
#4769=DIRECTION('',(0.,0.,1.));
#4770=DIRECTION('center_axis',(0.,0.,1.));
#4771=DIRECTION('ref_axis',(-0.707106781186549,0.707106781186546,0.));
#4772=DIRECTION('',(0.,0.,-1.));
#4773=DIRECTION('center_axis',(0.,0.,1.));
#4774=DIRECTION('ref_axis',(-0.707106781186549,0.707106781186546,0.));
#4775=DIRECTION('',(0.,0.,1.));
#4776=DIRECTION('center_axis',(-1.,0.,0.));
#4777=DIRECTION('ref_axis',(0.,-1.,0.));
#4778=DIRECTION('',(0.,-1.,0.));
#4779=DIRECTION('center_axis',(0.,1.,0.));
#4780=DIRECTION('ref_axis',(-1.,0.,0.));
#4781=DIRECTION('',(-1.,0.,0.));
#4782=DIRECTION('center_axis',(-1.,0.,0.));
#4783=DIRECTION('ref_axis',(0.,-1.,0.));
#4784=DIRECTION('',(0.,-1.,0.));
#4785=DIRECTION('center_axis',(1.,0.,0.));
#4786=DIRECTION('ref_axis',(0.,1.,0.));
#4787=DIRECTION('',(0.,1.,0.));
#4788=DIRECTION('center_axis',(0.,0.,1.));
#4789=DIRECTION('ref_axis',(1.,0.,0.));
#4790=DIRECTION('axis',(0.,0.,1.));
#4791=DIRECTION('refdir',(1.,0.,0.));
#4792=DIRECTION('center_axis',(0.,0.,-1.));
#4793=DIRECTION('ref_axis',(1.,0.,0.));
#4794=DIRECTION('center_axis',(0.,0.,-1.));
#4795=DIRECTION('ref_axis',(1.,0.,0.));
#4796=DIRECTION('',(0.,0.,-1.));
#4797=DIRECTION('center_axis',(0.,0.,1.));
#4798=DIRECTION('ref_axis',(1.,0.,0.));
#4799=DIRECTION('center_axis',(0.,0.,-1.));
#4800=DIRECTION('ref_axis',(1.,0.,0.));
#4801=DIRECTION('center_axis',(0.,0.,-1.));
#4802=DIRECTION('ref_axis',(1.,0.,0.));
#4803=DIRECTION('',(0.,0.,-1.));
#4804=DIRECTION('center_axis',(0.,0.,1.));
#4805=DIRECTION('ref_axis',(1.,0.,0.));
#4806=DIRECTION('center_axis',(0.,0.,-1.));
#4807=DIRECTION('ref_axis',(1.,0.,0.));
#4808=DIRECTION('center_axis',(0.,0.,-1.));
#4809=DIRECTION('ref_axis',(1.,0.,0.));
#4810=DIRECTION('',(0.,0.,-1.));
#4811=DIRECTION('center_axis',(0.,0.,1.));
#4812=DIRECTION('ref_axis',(1.,0.,0.));
#4813=DIRECTION('center_axis',(0.,0.,-1.));
#4814=DIRECTION('ref_axis',(1.,0.,0.));
#4815=DIRECTION('center_axis',(0.,0.,-1.));
#4816=DIRECTION('ref_axis',(1.,0.,0.));
#4817=DIRECTION('',(0.,0.,-1.));
#4818=DIRECTION('center_axis',(0.,0.,1.));
#4819=DIRECTION('ref_axis',(1.,0.,0.));
#4820=DIRECTION('center_axis',(0.,0.,-1.));
#4821=DIRECTION('ref_axis',(1.,0.,0.));
#4822=DIRECTION('center_axis',(0.,0.,-1.));
#4823=DIRECTION('ref_axis',(1.,0.,0.));
#4824=DIRECTION('',(0.,0.,-1.));
#4825=DIRECTION('center_axis',(0.,0.,1.));
#4826=DIRECTION('ref_axis',(1.,0.,0.));
#4827=DIRECTION('center_axis',(0.,0.,-1.));
#4828=DIRECTION('ref_axis',(1.,0.,0.));
#4829=DIRECTION('center_axis',(0.,0.,-1.));
#4830=DIRECTION('ref_axis',(1.,0.,0.));
#4831=DIRECTION('',(0.,0.,-1.));
#4832=DIRECTION('center_axis',(0.,0.,1.));
#4833=DIRECTION('ref_axis',(1.,0.,0.));
#4834=DIRECTION('center_axis',(0.,0.,-1.));
#4835=DIRECTION('ref_axis',(1.,0.,0.));
#4836=DIRECTION('center_axis',(0.,0.,-1.));
#4837=DIRECTION('ref_axis',(1.,0.,0.));
#4838=DIRECTION('',(0.,0.,-1.));
#4839=DIRECTION('center_axis',(0.,0.,1.));
#4840=DIRECTION('ref_axis',(1.,0.,0.));
#4841=DIRECTION('center_axis',(0.,0.,-1.));
#4842=DIRECTION('ref_axis',(1.,0.,0.));
#4843=DIRECTION('center_axis',(0.,0.,-1.));
#4844=DIRECTION('ref_axis',(1.,0.,0.));
#4845=DIRECTION('',(0.,0.,-1.));
#4846=DIRECTION('center_axis',(0.,0.,1.));
#4847=DIRECTION('ref_axis',(1.,0.,0.));
#4848=DIRECTION('center_axis',(0.,1.,0.));
#4849=DIRECTION('ref_axis',(1.,0.,0.));
#4850=DIRECTION('',(1.,0.,0.));
#4851=DIRECTION('',(0.,0.,-1.));
#4852=DIRECTION('',(-1.,0.,0.));
#4853=DIRECTION('',(0.,0.,-1.));
#4854=DIRECTION('center_axis',(-1.,0.,0.));
#4855=DIRECTION('ref_axis',(0.,1.,0.));
#4856=DIRECTION('',(0.,1.,0.));
#4857=DIRECTION('',(0.,0.,1.));
#4858=DIRECTION('',(0.,-1.,0.));
#4859=DIRECTION('center_axis',(0.,-1.,0.));
#4860=DIRECTION('ref_axis',(-1.,0.,0.));
#4861=DIRECTION('',(-1.,0.,0.));
#4862=DIRECTION('',(0.,0.,-1.));
#4863=DIRECTION('',(1.,0.,0.));
#4864=DIRECTION('',(0.,0.,-1.));
#4865=DIRECTION('center_axis',(1.,0.,0.));
#4866=DIRECTION('ref_axis',(0.,-1.,0.));
#4867=DIRECTION('',(0.,-1.,0.));
#4868=DIRECTION('',(0.,0.,1.));
#4869=DIRECTION('',(0.,1.,0.));
#4870=DIRECTION('center_axis',(1.,0.,0.));
#4871=DIRECTION('ref_axis',(0.,-1.,0.));
#4872=DIRECTION('',(0.,-1.,0.));
#4873=DIRECTION('',(0.,0.,-1.));
#4874=DIRECTION('',(0.,1.,0.));
#4875=DIRECTION('',(0.,0.,-1.));
#4876=DIRECTION('center_axis',(0.,1.,0.));
#4877=DIRECTION('ref_axis',(1.,0.,0.));
#4878=DIRECTION('',(1.,0.,0.));
#4879=DIRECTION('',(0.,0.,1.));
#4880=DIRECTION('',(-1.,0.,0.));
#4881=DIRECTION('center_axis',(0.,-1.,0.));
#4882=DIRECTION('ref_axis',(-1.,0.,0.));
#4883=DIRECTION('',(-1.,0.,0.));
#4884=DIRECTION('',(0.,0.,1.));
#4885=DIRECTION('',(1.,0.,0.));
#4886=DIRECTION('',(0.,0.,-1.));
#4887=DIRECTION('center_axis',(-1.,0.,0.));
#4888=DIRECTION('ref_axis',(0.,1.,0.));
#4889=DIRECTION('',(0.,1.,0.));
#4890=DIRECTION('',(0.,-1.,0.));
#4891=DIRECTION('',(0.,0.,-1.));
#4892=DIRECTION('center_axis',(-1.,0.,0.));
#4893=DIRECTION('ref_axis',(0.,-1.,0.));
#4894=DIRECTION('',(0.,-1.,0.));
#4895=DIRECTION('',(0.,-1.,0.));
#4896=DIRECTION('center_axis',(0.,1.,0.));
#4897=DIRECTION('ref_axis',(-1.,0.,0.));
#4898=DIRECTION('',(-1.,0.,0.));
#4899=DIRECTION('',(-1.,0.,0.));
#4900=DIRECTION('center_axis',(0.,0.,1.));
#4901=DIRECTION('ref_axis',(1.,0.,0.));
#4902=DIRECTION('',(1.,0.,0.));
#4903=DIRECTION('',(0.,1.,0.));
#4904=DIRECTION('center_axis',(0.,0.,1.));
#4905=DIRECTION('ref_axis',(1.,0.,0.));
#4906=DIRECTION('',(0.,1.,0.));
#4907=DIRECTION('',(1.,0.,0.));
#4908=DIRECTION('center_axis',(1.,0.,0.));
#4909=DIRECTION('ref_axis',(0.,1.,0.));
#4910=DIRECTION('center_axis',(0.,-1.,0.));
#4911=DIRECTION('ref_axis',(1.,0.,0.));
#4912=DIRECTION('axis',(0.,0.,1.));
#4913=DIRECTION('refdir',(1.,0.,0.));
#4914=DIRECTION('center_axis',(0.,0.,-1.));
#4915=DIRECTION('ref_axis',(1.,0.,0.));
#4916=DIRECTION('center_axis',(0.,0.,-1.));
#4917=DIRECTION('ref_axis',(1.,0.,0.));
#4918=DIRECTION('',(0.,0.,-1.));
#4919=DIRECTION('center_axis',(0.,0.,1.));
#4920=DIRECTION('ref_axis',(1.,0.,0.));
#4921=DIRECTION('center_axis',(0.,0.,-1.));
#4922=DIRECTION('ref_axis',(1.,0.,0.));
#4923=DIRECTION('center_axis',(0.,0.,-1.));
#4924=DIRECTION('ref_axis',(1.,0.,0.));
#4925=DIRECTION('',(0.,0.,-1.));
#4926=DIRECTION('center_axis',(0.,0.,1.));
#4927=DIRECTION('ref_axis',(1.,0.,0.));
#4928=DIRECTION('center_axis',(0.,0.,-1.));
#4929=DIRECTION('ref_axis',(1.,0.,0.));
#4930=DIRECTION('center_axis',(0.,0.,-1.));
#4931=DIRECTION('ref_axis',(1.,0.,0.));
#4932=DIRECTION('',(0.,0.,-1.));
#4933=DIRECTION('center_axis',(0.,0.,1.));
#4934=DIRECTION('ref_axis',(1.,0.,0.));
#4935=DIRECTION('center_axis',(0.,0.,-1.));
#4936=DIRECTION('ref_axis',(1.,0.,0.));
#4937=DIRECTION('center_axis',(0.,0.,-1.));
#4938=DIRECTION('ref_axis',(1.,0.,0.));
#4939=DIRECTION('',(0.,0.,-1.));
#4940=DIRECTION('center_axis',(0.,0.,1.));
#4941=DIRECTION('ref_axis',(1.,0.,0.));
#4942=DIRECTION('center_axis',(0.,1.,0.));
#4943=DIRECTION('ref_axis',(-1.,0.,0.));
#4944=DIRECTION('',(-1.,0.,0.));
#4945=DIRECTION('',(0.,0.,1.));
#4946=DIRECTION('',(-1.,0.,0.));
#4947=DIRECTION('',(0.,0.,1.));
#4948=DIRECTION('center_axis',(1.,0.,0.));
#4949=DIRECTION('ref_axis',(0.,1.,0.));
#4950=DIRECTION('',(0.,1.,0.));
#4951=DIRECTION('',(0.,1.,0.));
#4952=DIRECTION('',(0.,0.,1.));
#4953=DIRECTION('center_axis',(0.,-1.,0.));
#4954=DIRECTION('ref_axis',(1.,0.,0.));
#4955=DIRECTION('',(1.,0.,0.));
#4956=DIRECTION('',(1.,0.,0.));
#4957=DIRECTION('',(0.,0.,1.));
#4958=DIRECTION('center_axis',(-1.,0.,0.));
#4959=DIRECTION('ref_axis',(0.,-1.,0.));
#4960=DIRECTION('',(0.,-1.,0.));
#4961=DIRECTION('',(0.,-1.,0.));
#4962=DIRECTION('center_axis',(0.,0.,1.));
#4963=DIRECTION('ref_axis',(1.,0.,0.));
#4964=DIRECTION('center_axis',(0.,0.,1.));
#4965=DIRECTION('ref_axis',(1.,0.,0.));
#4966=DIRECTION('axis',(0.,0.,1.));
#4967=DIRECTION('refdir',(1.,0.,0.));
#4968=DIRECTION('center_axis',(0.,0.,-1.));
#4969=DIRECTION('ref_axis',(1.,0.,0.));
#4970=DIRECTION('center_axis',(0.,0.,-1.));
#4971=DIRECTION('ref_axis',(1.,0.,0.));
#4972=DIRECTION('',(0.,0.,-1.));
#4973=DIRECTION('center_axis',(0.,0.,1.));
#4974=DIRECTION('ref_axis',(1.,0.,0.));
#4975=DIRECTION('center_axis',(0.,0.,-1.));
#4976=DIRECTION('ref_axis',(1.,0.,0.));
#4977=DIRECTION('center_axis',(0.,0.,-1.));
#4978=DIRECTION('ref_axis',(1.,0.,0.));
#4979=DIRECTION('',(0.,0.,-1.));
#4980=DIRECTION('center_axis',(0.,0.,1.));
#4981=DIRECTION('ref_axis',(1.,0.,0.));
#4982=DIRECTION('center_axis',(0.,0.,-1.));
#4983=DIRECTION('ref_axis',(1.,0.,0.));
#4984=DIRECTION('center_axis',(0.,0.,-1.));
#4985=DIRECTION('ref_axis',(1.,0.,0.));
#4986=DIRECTION('',(0.,0.,-1.));
#4987=DIRECTION('center_axis',(0.,0.,1.));
#4988=DIRECTION('ref_axis',(1.,0.,0.));
#4989=DIRECTION('center_axis',(0.,0.,-1.));
#4990=DIRECTION('ref_axis',(1.,0.,0.));
#4991=DIRECTION('center_axis',(0.,0.,-1.));
#4992=DIRECTION('ref_axis',(1.,0.,0.));
#4993=DIRECTION('',(0.,0.,-1.));
#4994=DIRECTION('center_axis',(0.,0.,1.));
#4995=DIRECTION('ref_axis',(1.,0.,0.));
#4996=DIRECTION('center_axis',(0.,1.,0.));
#4997=DIRECTION('ref_axis',(-1.,0.,0.));
#4998=DIRECTION('',(-1.,0.,0.));
#4999=DIRECTION('',(0.,0.,1.));
#5000=DIRECTION('',(-1.,0.,0.));
#5001=DIRECTION('',(0.,0.,1.));
#5002=DIRECTION('center_axis',(1.,0.,0.));
#5003=DIRECTION('ref_axis',(0.,1.,0.));
#5004=DIRECTION('',(0.,1.,0.));
#5005=DIRECTION('',(0.,1.,0.));
#5006=DIRECTION('',(0.,0.,1.));
#5007=DIRECTION('center_axis',(0.,-1.,0.));
#5008=DIRECTION('ref_axis',(1.,0.,0.));
#5009=DIRECTION('',(1.,0.,0.));
#5010=DIRECTION('',(1.,0.,0.));
#5011=DIRECTION('',(0.,0.,1.));
#5012=DIRECTION('center_axis',(-1.,0.,0.));
#5013=DIRECTION('ref_axis',(0.,-1.,0.));
#5014=DIRECTION('',(0.,-1.,0.));
#5015=DIRECTION('',(0.,-1.,0.));
#5016=DIRECTION('center_axis',(0.,0.,1.));
#5017=DIRECTION('ref_axis',(1.,0.,0.));
#5018=DIRECTION('center_axis',(0.,0.,1.));
#5019=DIRECTION('ref_axis',(1.,0.,0.));
#5020=DIRECTION('axis',(0.,0.,1.));
#5021=DIRECTION('refdir',(1.,0.,0.));
#5022=DIRECTION('center_axis',(0.,1.,0.));
#5023=DIRECTION('ref_axis',(-1.,0.,0.));
#5024=DIRECTION('',(-1.,0.,0.));
#5025=DIRECTION('',(0.,0.,1.));
#5026=DIRECTION('',(-1.,0.,0.));
#5027=DIRECTION('',(0.,0.,1.));
#5028=DIRECTION('center_axis',(1.,0.,0.));
#5029=DIRECTION('ref_axis',(0.,1.,0.));
#5030=DIRECTION('',(0.,1.,0.));
#5031=DIRECTION('',(0.,1.,0.));
#5032=DIRECTION('',(0.,0.,1.));
#5033=DIRECTION('center_axis',(0.,-1.,0.));
#5034=DIRECTION('ref_axis',(1.,0.,0.));
#5035=DIRECTION('',(1.,0.,0.));
#5036=DIRECTION('',(1.,0.,0.));
#5037=DIRECTION('',(0.,0.,1.));
#5038=DIRECTION('center_axis',(-1.,0.,0.));
#5039=DIRECTION('ref_axis',(0.,-1.,0.));
#5040=DIRECTION('',(0.,-1.,0.));
#5041=DIRECTION('',(0.,-1.,0.));
#5042=DIRECTION('center_axis',(0.,0.,1.));
#5043=DIRECTION('ref_axis',(1.,0.,0.));
#5044=DIRECTION('center_axis',(0.,0.,1.));
#5045=DIRECTION('ref_axis',(1.,0.,0.));
#5046=DIRECTION('axis',(0.,0.,1.));
#5047=DIRECTION('refdir',(1.,0.,0.));
#5048=DIRECTION('center_axis',(0.707106781186548,0.707106781186548,0.));
#5049=DIRECTION('ref_axis',(-0.707106781186548,0.707106781186548,0.));
#5050=DIRECTION('',(-0.707106781186547,0.707106781186547,0.));
#5051=DIRECTION('',(0.,0.,1.));
#5052=DIRECTION('',(-0.707106781186547,0.707106781186547,0.));
#5053=DIRECTION('',(0.,0.,1.));
#5054=DIRECTION('center_axis',(0.,-1.,0.));
#5055=DIRECTION('ref_axis',(1.,0.,0.));
#5056=DIRECTION('',(1.,0.,0.));
#5057=DIRECTION('',(1.,0.,0.));
#5058=DIRECTION('',(0.,0.,1.));
#5059=DIRECTION('center_axis',(-1.,0.,0.));
#5060=DIRECTION('ref_axis',(0.,-1.,0.));
#5061=DIRECTION('',(0.,-1.,0.));
#5062=DIRECTION('',(0.,-1.,0.));
#5063=DIRECTION('center_axis',(0.,0.,1.));
#5064=DIRECTION('ref_axis',(1.,0.,0.));
#5065=DIRECTION('center_axis',(0.,0.,1.));
#5066=DIRECTION('ref_axis',(1.,0.,0.));
#5067=DIRECTION('axis',(0.,0.,1.));
#5068=DIRECTION('refdir',(1.,0.,0.));
#5069=DIRECTION('center_axis',(0.,0.,1.));
#5070=DIRECTION('ref_axis',(0.938002329630376,0.346628950908588,0.));
#5071=DIRECTION('',(0.,0.,-1.));
#5072=DIRECTION('center_axis',(0.,0.,1.));
#5073=DIRECTION('ref_axis',(1.,0.,0.));
#5074=DIRECTION('center_axis',(0.,0.,1.));
#5075=DIRECTION('ref_axis',(1.,0.,0.));
#5076=DIRECTION('',(0.,0.,-1.));
#5077=DIRECTION('center_axis',(0.,0.,1.));
#5078=DIRECTION('ref_axis',(1.,0.,0.));
#5079=DIRECTION('',(0.,0.,-1.));
#5080=DIRECTION('center_axis',(0.,0.,1.));
#5081=DIRECTION('ref_axis',(1.,0.,0.));
#5082=DIRECTION('',(0.,0.,-1.));
#5083=DIRECTION('center_axis',(0.,0.,1.));
#5084=DIRECTION('ref_axis',(1.,0.,0.));
#5085=DIRECTION('',(0.,0.,-1.));
#5086=DIRECTION('center_axis',(0.,0.,1.));
#5087=DIRECTION('ref_axis',(1.,0.,0.));
#5088=DIRECTION('',(0.,0.,-1.));
#5089=DIRECTION('center_axis',(0.,0.,1.));
#5090=DIRECTION('ref_axis',(1.,0.,0.));
#5091=DIRECTION('',(0.,0.,-1.));
#5092=DIRECTION('center_axis',(0.,0.,1.));
#5093=DIRECTION('ref_axis',(1.,0.,0.));
#5094=DIRECTION('',(0.,0.,-1.));
#5095=DIRECTION('center_axis',(0.,0.,1.));
#5096=DIRECTION('ref_axis',(-0.346901083835764,-0.937901720882083,0.));
#5097=DIRECTION('',(0.,0.,-1.));
#5098=DIRECTION('center_axis',(0.,0.,1.));
#5099=DIRECTION('ref_axis',(1.,0.,0.));
#5100=DIRECTION('center_axis',(0.,0.,1.));
#5101=DIRECTION('ref_axis',(1.,4.65526718641507E-14,0.));
#5102=DIRECTION('',(1.22464679914735E-16,5.71605565684554E-30,1.));
#5103=DIRECTION('center_axis',(0.,0.,-1.));
#5104=DIRECTION('ref_axis',(1.,4.65526718641507E-14,0.));
#5105=DIRECTION('center_axis',(0.,0.,1.));
#5106=DIRECTION('ref_axis',(1.,4.65526718641507E-14,0.));
#5107=DIRECTION('',(1.22464679914735E-16,5.71605565684554E-30,1.));
#5108=DIRECTION('center_axis',(0.,0.,1.));
#5109=DIRECTION('ref_axis',(1.,4.65526718641507E-14,0.));
#5110=DIRECTION('',(1.22464679914735E-16,5.71605565684554E-30,1.));
#5111=DIRECTION('center_axis',(0.,0.,1.));
#5112=DIRECTION('ref_axis',(1.,4.65526718641507E-14,0.));
#5113=DIRECTION('',(1.22464679914735E-16,5.71605565684554E-30,1.));
#5114=DIRECTION('center_axis',(0.,0.,1.));
#5115=DIRECTION('ref_axis',(1.,4.65526718641507E-14,0.));
#5116=DIRECTION('',(1.22464679914735E-16,5.71605565684554E-30,1.));
#5117=DIRECTION('center_axis',(0.,0.,1.));
#5118=DIRECTION('ref_axis',(1.,4.65526718641507E-14,0.));
#5119=DIRECTION('',(1.22464679914735E-16,5.71605565684554E-30,1.));
#5120=DIRECTION('center_axis',(0.,0.,1.));
#5121=DIRECTION('ref_axis',(1.,4.65526718641507E-14,0.));
#5122=DIRECTION('',(1.22464679914735E-16,5.71605565684554E-30,1.));
#5123=DIRECTION('center_axis',(0.,0.,1.));
#5124=DIRECTION('ref_axis',(1.,4.65526718641507E-14,0.));
#5125=DIRECTION('',(1.22464679914735E-16,5.71605565684554E-30,1.));
#5126=DIRECTION('center_axis',(0.,0.,1.));
#5127=DIRECTION('ref_axis',(-0.609180499130755,0.793031600554987,0.));
#5128=DIRECTION('',(1.22464679914735E-16,5.71605565684554E-30,1.));
#5129=DIRECTION('center_axis',(0.,0.,1.));
#5130=DIRECTION('ref_axis',(1.,4.65526718641507E-14,0.));
#5131=DIRECTION('center_axis',(0.,0.,1.));
#5132=DIRECTION('ref_axis',(1.,4.65526718641507E-14,0.));
#5133=DIRECTION('center_axis',(0.,0.,1.));
#5134=DIRECTION('ref_axis',(1.,0.,0.));
#5135=DIRECTION('center_axis',(0.,0.,1.));
#5136=DIRECTION('ref_axis',(1.,0.,0.));
#5137=DIRECTION('center_axis',(0.,0.,1.));
#5138=DIRECTION('ref_axis',(1.,0.,0.));
#5139=DIRECTION('center_axis',(0.,0.,1.));
#5140=DIRECTION('ref_axis',(1.,0.,0.));
#5141=DIRECTION('center_axis',(0.,0.,1.));
#5142=DIRECTION('ref_axis',(1.,0.,0.));
#5143=DIRECTION('center_axis',(0.,0.,1.));
#5144=DIRECTION('ref_axis',(1.,0.,0.));
#5145=DIRECTION('center_axis',(0.,0.,1.));
#5146=DIRECTION('ref_axis',(1.,0.,0.));
#5147=DIRECTION('center_axis',(0.,0.,-1.));
#5148=DIRECTION('ref_axis',(1.,0.,0.));
#5149=DIRECTION('center_axis',(0.,0.,1.));
#5150=DIRECTION('ref_axis',(1.,0.,0.));
#5151=DIRECTION('',(0.,0.,-1.));
#5152=DIRECTION('center_axis',(0.,0.,1.));
#5153=DIRECTION('ref_axis',(1.,0.,0.));
#5154=DIRECTION('',(0.,0.,-1.));
#5155=DIRECTION('center_axis',(0.,0.,1.));
#5156=DIRECTION('ref_axis',(1.,0.,0.));
#5157=DIRECTION('center_axis',(0.,0.,1.));
#5158=DIRECTION('ref_axis',(1.,0.,0.));
#5159=DIRECTION('center_axis',(0.,0.,1.));
#5160=DIRECTION('ref_axis',(1.,0.,0.));
#5161=DIRECTION('center_axis',(0.,0.,1.));
#5162=DIRECTION('ref_axis',(1.,0.,0.));
#5163=DIRECTION('center_axis',(0.,0.,1.));
#5164=DIRECTION('ref_axis',(1.,0.,0.));
#5165=DIRECTION('',(0.,0.,-1.));
#5166=DIRECTION('center_axis',(0.,0.,1.));
#5167=DIRECTION('ref_axis',(1.,0.,0.));
#5168=DIRECTION('center_axis',(0.,0.,1.));
#5169=DIRECTION('ref_axis',(1.,0.,0.));
#5170=DIRECTION('',(0.,0.,-1.));
#5171=DIRECTION('center_axis',(0.,0.,1.));
#5172=DIRECTION('ref_axis',(1.,0.,0.));
#5173=DIRECTION('axis',(0.,0.,1.));
#5174=DIRECTION('refdir',(1.,0.,0.));
#5175=DIRECTION('center_axis',(0.,0.,1.));
#5176=DIRECTION('ref_axis',(1.,0.,0.));
#5177=DIRECTION('',(0.,0.,-1.));
#5178=DIRECTION('center_axis',(0.,0.,-1.));
#5179=DIRECTION('ref_axis',(1.,0.,0.));
#5180=DIRECTION('center_axis',(0.,0.,1.));
#5181=DIRECTION('ref_axis',(1.,0.,0.));
#5182=DIRECTION('',(0.,0.,-1.));
#5183=DIRECTION('center_axis',(0.,0.,1.));
#5184=DIRECTION('ref_axis',(1.,0.,0.));
#5185=DIRECTION('',(0.,0.,-1.));
#5186=DIRECTION('center_axis',(0.,0.,1.));
#5187=DIRECTION('ref_axis',(1.,0.,0.));
#5188=DIRECTION('',(0.,0.,-1.));
#5189=DIRECTION('center_axis',(0.,0.,1.));
#5190=DIRECTION('ref_axis',(1.,0.,0.));
#5191=DIRECTION('',(0.,0.,-1.));
#5192=DIRECTION('center_axis',(0.,0.,1.));
#5193=DIRECTION('ref_axis',(1.,0.,0.));
#5194=DIRECTION('',(0.,0.,-1.));
#5195=DIRECTION('center_axis',(0.,0.,1.));
#5196=DIRECTION('ref_axis',(1.,0.,0.));
#5197=DIRECTION('',(0.,0.,-1.));
#5198=DIRECTION('center_axis',(0.,0.,1.));
#5199=DIRECTION('ref_axis',(1.,0.,0.));
#5200=DIRECTION('',(0.,0.,-1.));
#5201=DIRECTION('center_axis',(0.,0.,1.));
#5202=DIRECTION('ref_axis',(1.,0.,0.));
#5203=DIRECTION('',(0.,0.,-1.));
#5204=DIRECTION('center_axis',(0.,0.,1.));
#5205=DIRECTION('ref_axis',(1.,0.,0.));
#5206=DIRECTION('',(0.,0.,-1.));
#5207=DIRECTION('center_axis',(0.,0.,1.));
#5208=DIRECTION('ref_axis',(1.,0.,0.));
#5209=DIRECTION('',(0.,0.,-1.));
#5210=DIRECTION('center_axis',(0.,0.,1.));
#5211=DIRECTION('ref_axis',(0.997344302588954,-0.0728309144069492,0.));
#5212=DIRECTION('',(0.,0.,1.));
#5213=DIRECTION('center_axis',(0.,0.,-1.));
#5214=DIRECTION('ref_axis',(1.,7.52212518638754E-14,0.));
#5215=DIRECTION('center_axis',(0.,0.,1.));
#5216=DIRECTION('ref_axis',(1.,7.52212518638754E-14,0.));
#5217=DIRECTION('',(0.,0.,1.));
#5218=DIRECTION('center_axis',(0.,0.,1.));
#5219=DIRECTION('ref_axis',(1.,7.52212518638754E-14,0.));
#5220=DIRECTION('',(0.,0.,1.));
#5221=DIRECTION('center_axis',(0.,0.,1.));
#5222=DIRECTION('ref_axis',(1.,7.52212518638754E-14,0.));
#5223=DIRECTION('',(0.,0.,1.));
#5224=DIRECTION('center_axis',(0.,0.,1.));
#5225=DIRECTION('ref_axis',(1.,7.52212518638754E-14,0.));
#5226=DIRECTION('',(0.,0.,1.));
#5227=DIRECTION('center_axis',(0.,0.,1.));
#5228=DIRECTION('ref_axis',(1.,7.52212518638754E-14,0.));
#5229=DIRECTION('',(0.,0.,1.));
#5230=DIRECTION('center_axis',(0.,0.,1.));
#5231=DIRECTION('ref_axis',(1.,7.52212518638754E-14,0.));
#5232=DIRECTION('',(0.,0.,1.));
#5233=DIRECTION('center_axis',(0.,0.,1.));
#5234=DIRECTION('ref_axis',(1.,7.52212518638754E-14,0.));
#5235=DIRECTION('',(0.,0.,1.));
#5236=DIRECTION('center_axis',(0.,0.,1.));
#5237=DIRECTION('ref_axis',(1.,7.52212518638754E-14,0.));
#5238=DIRECTION('',(0.,0.,1.));
#5239=DIRECTION('center_axis',(0.,0.,1.));
#5240=DIRECTION('ref_axis',(1.,7.52212518638754E-14,0.));
#5241=DIRECTION('',(0.,0.,1.));
#5242=DIRECTION('center_axis',(0.,0.,1.));
#5243=DIRECTION('ref_axis',(1.,7.52212518638754E-14,0.));
#5244=DIRECTION('',(0.,0.,1.));
#5245=DIRECTION('center_axis',(0.,0.,-1.));
#5246=DIRECTION('ref_axis',(1.,0.,0.));
#5247=DIRECTION('center_axis',(0.,0.,-1.));
#5248=DIRECTION('ref_axis',(1.,0.,0.));
#5249=DIRECTION('',(0.707106781186548,8.65956056235494E-17,0.707106781186547));
#5250=DIRECTION('center_axis',(0.,0.,1.));
#5251=DIRECTION('ref_axis',(1.,0.,0.));
#5252=DIRECTION('center_axis',(0.,0.,1.));
#5253=DIRECTION('ref_axis',(1.,7.52212518638754E-14,0.));
#5254=DIRECTION('center_axis',(0.,0.,-1.));
#5255=DIRECTION('ref_axis',(1.,7.52212518638754E-14,0.));
#5256=DIRECTION('center_axis',(0.,0.,1.));
#5257=DIRECTION('ref_axis',(1.,0.,0.));
#5258=DIRECTION('center_axis',(-1.92296268638356E-16,-1.,0.));
#5259=DIRECTION('ref_axis',(1.,-1.92296268638356E-16,0.));
#5260=DIRECTION('',(1.,-1.92296268638356E-16,0.));
#5261=DIRECTION('',(0.,0.,1.));
#5262=DIRECTION('',(1.,-1.92296268638356E-16,0.));
#5263=DIRECTION('',(0.,0.,1.));
#5264=DIRECTION('center_axis',(-0.866025403784439,-0.5,0.));
#5265=DIRECTION('ref_axis',(0.5,-0.866025403784439,0.));
#5266=DIRECTION('',(0.5,-0.866025403784439,0.));
#5267=DIRECTION('',(0.,0.,1.));
#5268=DIRECTION('',(0.5,-0.866025403784439,0.));
#5269=DIRECTION('center_axis',(-0.866025403784439,0.5,0.));
#5270=DIRECTION('ref_axis',(-0.5,-0.866025403784438,0.));
#5271=DIRECTION('',(-0.5,-0.866025403784438,0.));
#5272=DIRECTION('',(0.,0.,1.));
#5273=DIRECTION('',(-0.5,-0.866025403784439,0.));
#5274=DIRECTION('center_axis',(1.92296268638356E-16,1.,0.));
#5275=DIRECTION('ref_axis',(-1.,1.92296268638356E-16,0.));
#5276=DIRECTION('',(-1.,1.92296268638356E-16,0.));
#5277=DIRECTION('',(0.,0.,1.));
#5278=DIRECTION('',(-1.,1.92296268638356E-16,0.));
#5279=DIRECTION('center_axis',(0.866025403784439,0.5,0.));
#5280=DIRECTION('ref_axis',(-0.5,0.866025403784439,0.));
#5281=DIRECTION('',(-0.5,0.866025403784439,0.));
#5282=DIRECTION('',(0.,0.,1.));
#5283=DIRECTION('',(-0.5,0.866025403784439,0.));
#5284=DIRECTION('center_axis',(0.866025403784439,-0.5,0.));
#5285=DIRECTION('ref_axis',(0.5,0.866025403784439,0.));
#5286=DIRECTION('',(0.5,0.866025403784439,0.));
#5287=DIRECTION('',(0.5,0.866025403784439,0.));
#5288=DIRECTION('center_axis',(0.,0.,1.));
#5289=DIRECTION('ref_axis',(1.,0.,0.));
#5290=DIRECTION('center_axis',(0.,0.,1.));
#5291=DIRECTION('ref_axis',(1.,0.,0.));
#5292=DIRECTION('center_axis',(0.,0.,1.));
#5293=DIRECTION('ref_axis',(1.,0.,0.));
#5294=DIRECTION('center_axis',(0.,0.,1.));
#5295=DIRECTION('ref_axis',(1.,0.,0.));
#5296=DIRECTION('',(0.,0.,-1.));
#5297=DIRECTION('center_axis',(0.,0.,1.));
#5298=DIRECTION('ref_axis',(1.,0.,0.));
#5299=DIRECTION('center_axis',(0.,0.,1.));
#5300=DIRECTION('ref_axis',(1.,0.,0.));
#5301=DIRECTION('center_axis',(0.,0.,1.));
#5302=DIRECTION('ref_axis',(1.,0.,0.));
#5303=DIRECTION('',(0.,0.,1.));
#5304=DIRECTION('',(1.,0.,0.));
#5305=DIRECTION('',(1.,0.,0.));
#5306=DIRECTION('',(0.,1.,0.));
#5307=DIRECTION('',(0.,0.,1.));
#5308=DIRECTION('',(1.,0.,0.));
#5309=DIRECTION('',(0.,0.,1.));
#5310=DIRECTION('',(1.,0.,0.));
#5311=DIRECTION('',(0.,0.,1.));
#5312=DIRECTION('',(1.,0.,0.));
#5313=DIRECTION('',(0.,1.,0.));
#5314=DIRECTION('',(1.,0.,0.));
#5315=DIRECTION('',(1.,0.,0.));
#5316=DIRECTION('',(0.,1.,0.));
#5317=DIRECTION('',(1.,0.,0.));
#5318=DIRECTION('',(0.,1.,0.));
#5319=DIRECTION('',(1.,0.,0.));
#5320=DIRECTION('',(0.,1.,0.));
#5321=DIRECTION('',(1.,0.,0.));
#5322=DIRECTION('',(0.,1.,0.));
#5323=DIRECTION('',(1.,0.,0.));
#5324=DIRECTION('',(0.,1.,0.));
#5325=DIRECTION('',(1.,0.,0.));
#5326=DIRECTION('',(0.,1.,0.));
#5327=DIRECTION('',(0.,1.,0.));
#5328=DIRECTION('',(1.,0.,0.));
#5329=DIRECTION('',(0.,1.,0.));
#5330=DIRECTION('',(1.,0.,0.));
#5331=DIRECTION('',(0.,1.,0.));
#5332=DIRECTION('',(1.,0.,0.));
#5333=DIRECTION('',(0.,0.,1.));
#5334=DIRECTION('',(1.,0.,0.));
#5335=DIRECTION('',(0.,0.,1.));
#5336=DIRECTION('',(1.,0.,0.));
#5337=DIRECTION('',(0.,0.,1.));
#5338=DIRECTION('',(1.,0.,0.));
#5339=DIRECTION('',(0.,0.,1.));
#5340=DIRECTION('',(1.,0.,0.));
#5341=DIRECTION('',(0.,1.,0.));
#5342=DIRECTION('',(1.,0.,0.));
#5343=DIRECTION('',(0.,0.,1.));
#5344=DIRECTION('',(1.,0.,0.));
#5345=DIRECTION('',(0.,-1.22464679914735E-16,-1.));
#5346=DIRECTION('',(-0.984807753012208,-0.17364817766693,2.12657684957577E-17));
#5347=DIRECTION('',(1.,0.,0.));
#5348=DIRECTION('',(0.,1.,0.));
#5349=DIRECTION('',(0.,0.,1.));
#5350=DIRECTION('',(1.,0.,0.));
#5351=DIRECTION('',(0.,0.,1.));
#5352=DIRECTION('',(1.,0.,0.));
#5353=DIRECTION('',(0.,0.,1.));
#5354=DIRECTION('',(1.,0.,0.));
#5355=DIRECTION('',(0.,0.,1.));
#5356=DIRECTION('',(1.,0.,0.));
#5357=DIRECTION('',(0.,0.,1.));
#5358=DIRECTION('',(1.,0.,0.));
#5359=DIRECTION('',(0.,0.,1.));
#5360=DIRECTION('',(1.,0.,0.));
#5361=DIRECTION('',(0.,0.,1.));
#5362=DIRECTION('',(1.,0.,0.));
#5363=DIRECTION('',(0.,0.,1.));
#5364=DIRECTION('',(1.,0.,0.));
#5365=DIRECTION('',(0.,0.,1.));
#5366=DIRECTION('',(1.,0.,0.));
#5367=DIRECTION('',(0.,0.,1.));
#5368=DIRECTION('',(1.,0.,0.));
#5369=DIRECTION('',(0.,-1.,0.));
#5370=DIRECTION('',(-1.,0.,0.));
#5371=DIRECTION('',(0.,-1.,0.));
#5372=DIRECTION('',(1.,0.,0.));
#5373=DIRECTION('',(0.,1.,0.));
#5374=DIRECTION('',(-1.,0.,0.));
#5375=DIRECTION('',(0.,0.,1.));
#5376=DIRECTION('',(1.,0.,0.));
#5377=DIRECTION('',(0.,0.,1.));
#5378=DIRECTION('',(1.,0.,0.));
#5379=DIRECTION('',(0.,0.,1.));
#5380=DIRECTION('',(1.,0.,0.));
#5381=DIRECTION('',(0.,0.,1.));
#5382=DIRECTION('',(1.,0.,0.));
#5383=DIRECTION('',(0.,0.,1.));
#5384=DIRECTION('',(1.,0.,0.));
#5385=DIRECTION('',(0.,0.,1.));
#5386=DIRECTION('',(1.,0.,0.));
#5387=DIRECTION('',(0.,0.,1.));
#5388=DIRECTION('',(1.,0.,0.));
#5389=DIRECTION('',(0.,-1.22464679914735E-16,-1.));
#5390=DIRECTION('',(-0.984807753012208,-0.17364817766693,2.12657684957577E-17));
#5391=DIRECTION('',(0.,-1.22464679914735E-16,-1.));
#5392=DIRECTION('',(-0.984807753012208,-0.17364817766693,2.12657684957577E-17));
#5393=DIRECTION('',(0.,-1.22464679914735E-16,-1.));
#5394=DIRECTION('',(-0.984807753012208,-0.17364817766693,2.12657684957577E-17));
#5395=DIRECTION('',(0.,-1.22464679914735E-16,-1.));
#5396=DIRECTION('',(-0.984807753012208,-0.17364817766693,2.12657684957577E-17));
#5397=DIRECTION('',(0.,-1.22464679914735E-16,-1.));
#5398=DIRECTION('',(-0.984807753012208,-0.17364817766693,2.12657684957577E-17));
#5399=DIRECTION('',(0.,-1.22464679914735E-16,-1.));
#5400=DIRECTION('',(-0.984807753012208,-0.17364817766693,2.12657684957577E-17));
#5401=DIRECTION('',(0.,-1.22464679914735E-16,-1.));
#5402=DIRECTION('',(-0.984807753012208,-0.17364817766693,2.12657684957577E-17));
#5403=CARTESIAN_POINT('',(0.,0.,0.));
#5404=CARTESIAN_POINT('',(0.,0.,0.));
#5405=CARTESIAN_POINT('Origin',(-19.,-19.,0.));
#5406=CARTESIAN_POINT('',(-19.,-20.,1000.));
#5407=CARTESIAN_POINT('',(-20.,-19.,1000.));
#5408=CARTESIAN_POINT('Origin',(-19.,-19.,1000.));
#5409=CARTESIAN_POINT('',(-20.,-19.,0.));
#5410=CARTESIAN_POINT('',(-20.,-19.,0.));
#5411=CARTESIAN_POINT('',(-19.,-20.,0.));
#5412=CARTESIAN_POINT('Origin',(-19.,-19.,0.));
#5413=CARTESIAN_POINT('',(-19.,-20.,0.));
#5414=CARTESIAN_POINT('Origin',(-20.,20.,0.));
#5415=CARTESIAN_POINT('',(-20.,19.,1000.));
#5416=CARTESIAN_POINT('',(-20.,20.,1000.));
#5417=CARTESIAN_POINT('',(-20.,19.,0.));
#5418=CARTESIAN_POINT('',(-20.,19.,0.));
#5419=CARTESIAN_POINT('',(-20.,20.,0.));
#5420=CARTESIAN_POINT('Origin',(0.,0.,1000.));
#5421=CARTESIAN_POINT('',(19.,-20.,1000.));
#5422=CARTESIAN_POINT('',(-20.,-20.,1000.));
#5423=CARTESIAN_POINT('',(20.,-19.,1000.));
#5424=CARTESIAN_POINT('Origin',(19.,-19.,1000.));
#5425=CARTESIAN_POINT('',(20.,19.,1000.));
#5426=CARTESIAN_POINT('',(20.,-20.,1000.));
#5427=CARTESIAN_POINT('',(19.,20.,1000.));
#5428=CARTESIAN_POINT('Origin',(19.,19.,1000.));
#5429=CARTESIAN_POINT('',(-19.,20.,1000.));
#5430=CARTESIAN_POINT('',(20.,20.,1000.));
#5431=CARTESIAN_POINT('Origin',(-19.,19.,1000.));
#5432=CARTESIAN_POINT('',(-16.,-15.,1000.));
#5433=CARTESIAN_POINT('',(-16.,15.,1000.));
#5434=CARTESIAN_POINT('',(-16.,16.,1000.));
#5435=CARTESIAN_POINT('',(-15.,16.,1000.));
#5436=CARTESIAN_POINT('Origin',(-15.,15.,1000.));
#5437=CARTESIAN_POINT('',(15.,16.,1000.));
#5438=CARTESIAN_POINT('',(16.,16.,1000.));
#5439=CARTESIAN_POINT('',(16.,15.,1000.));
#5440=CARTESIAN_POINT('Origin',(15.,15.,1000.));
#5441=CARTESIAN_POINT('',(16.,-15.,1000.));
#5442=CARTESIAN_POINT('',(16.,-16.,1000.));
#5443=CARTESIAN_POINT('',(15.,-16.,1000.));
#5444=CARTESIAN_POINT('Origin',(15.,-15.,1000.));
#5445=CARTESIAN_POINT('',(-15.,-16.,1000.));
#5446=CARTESIAN_POINT('',(-16.,-16.,1000.));
#5447=CARTESIAN_POINT('Origin',(-15.,-15.,1000.));
#5448=CARTESIAN_POINT('Origin',(19.,-19.,0.));
#5449=CARTESIAN_POINT('',(19.,-20.,0.));
#5450=CARTESIAN_POINT('',(19.,-20.,0.));
#5451=CARTESIAN_POINT('',(20.,-19.,0.));
#5452=CARTESIAN_POINT('Origin',(19.,-19.,0.));
#5453=CARTESIAN_POINT('',(20.,-19.,0.));
#5454=CARTESIAN_POINT('Origin',(20.,-20.,0.));
#5455=CARTESIAN_POINT('',(20.,19.,0.));
#5456=CARTESIAN_POINT('',(20.,-20.,0.));
#5457=CARTESIAN_POINT('',(20.,19.,0.));
#5458=CARTESIAN_POINT('Origin',(19.,19.,0.));
#5459=CARTESIAN_POINT('',(19.,20.,0.));
#5460=CARTESIAN_POINT('Origin',(19.,19.,0.));
#5461=CARTESIAN_POINT('',(19.,20.,0.));
#5462=CARTESIAN_POINT('Origin',(-19.,19.,0.));
#5463=CARTESIAN_POINT('',(-19.,20.,0.));
#5464=CARTESIAN_POINT('',(-19.,20.,0.));
#5465=CARTESIAN_POINT('Origin',(-19.,19.,0.));
#5466=CARTESIAN_POINT('Origin',(-15.,15.,0.));
#5467=CARTESIAN_POINT('',(-16.,15.,0.));
#5468=CARTESIAN_POINT('',(-15.,16.,0.));
#5469=CARTESIAN_POINT('Origin',(-15.,15.,0.));
#5470=CARTESIAN_POINT('',(-15.,16.,0.));
#5471=CARTESIAN_POINT('',(-16.,15.,0.));
#5472=CARTESIAN_POINT('Origin',(-16.,16.,0.));
#5473=CARTESIAN_POINT('',(15.,16.,0.));
#5474=CARTESIAN_POINT('',(16.,16.,0.));
#5475=CARTESIAN_POINT('',(15.,16.,0.));
#5476=CARTESIAN_POINT('Origin',(15.,15.,0.));
#5477=CARTESIAN_POINT('',(16.,15.,0.));
#5478=CARTESIAN_POINT('Origin',(15.,15.,0.));
#5479=CARTESIAN_POINT('',(16.,15.,0.));
#5480=CARTESIAN_POINT('Origin',(16.,16.,0.));
#5481=CARTESIAN_POINT('',(16.,-15.,0.));
#5482=CARTESIAN_POINT('',(16.,-16.,0.));
#5483=CARTESIAN_POINT('',(16.,-15.,0.));
#5484=CARTESIAN_POINT('Origin',(15.,-15.,0.));
#5485=CARTESIAN_POINT('',(15.,-16.,0.));
#5486=CARTESIAN_POINT('Origin',(15.,-15.,0.));
#5487=CARTESIAN_POINT('',(15.,-16.,0.));
#5488=CARTESIAN_POINT('Origin',(16.,-16.,0.));
#5489=CARTESIAN_POINT('',(-15.,-16.,0.));
#5490=CARTESIAN_POINT('',(-16.,-16.,0.));
#5491=CARTESIAN_POINT('',(-15.,-16.,0.));
#5492=CARTESIAN_POINT('Origin',(-15.,-15.,0.));
#5493=CARTESIAN_POINT('',(-16.,-15.,0.));
#5494=CARTESIAN_POINT('Origin',(-15.,-15.,0.));
#5495=CARTESIAN_POINT('',(-16.,-15.,0.));
#5496=CARTESIAN_POINT('Origin',(-16.,-16.,0.));
#5497=CARTESIAN_POINT('',(-16.,16.,0.));
#5498=CARTESIAN_POINT('Origin',(20.,20.,0.));
#5499=CARTESIAN_POINT('',(20.,20.,0.));
#5500=CARTESIAN_POINT('Origin',(-20.,-20.,0.));
#5501=CARTESIAN_POINT('',(-20.,-20.,0.));
#5502=CARTESIAN_POINT('Origin',(0.,0.,0.));
#5503=CARTESIAN_POINT('',(0.,0.,0.));
#5504=CARTESIAN_POINT('Origin',(0.,18.,60.));
#5505=CARTESIAN_POINT('',(6.12323399573677E-16,20.,55.));
#5506=CARTESIAN_POINT('Origin',(0.,20.,60.));
#5507=CARTESIAN_POINT('',(6.12323399573677E-16,16.,55.));
#5508=CARTESIAN_POINT('',(6.12323399573677E-16,18.,55.));
#5509=CARTESIAN_POINT('Origin',(0.,16.,60.));
#5510=CARTESIAN_POINT('Origin',(0.,18.,660.));
#5511=CARTESIAN_POINT('',(6.12323399573677E-16,20.,655.));
#5512=CARTESIAN_POINT('Origin',(0.,20.,660.));
#5513=CARTESIAN_POINT('',(6.12323399573677E-16,16.,655.));
#5514=CARTESIAN_POINT('',(6.12323399573677E-16,18.,655.));
#5515=CARTESIAN_POINT('Origin',(0.,16.,660.));
#5516=CARTESIAN_POINT('Origin',(-19.,-19.,0.));
#5517=CARTESIAN_POINT('',(-19.,-20.,720.));
#5518=CARTESIAN_POINT('',(-20.,-19.,720.));
#5519=CARTESIAN_POINT('Origin',(-19.,-19.,720.));
#5520=CARTESIAN_POINT('',(-20.,-19.,0.));
#5521=CARTESIAN_POINT('',(-20.,-19.,0.));
#5522=CARTESIAN_POINT('',(-19.,-20.,0.));
#5523=CARTESIAN_POINT('Origin',(-19.,-19.,0.));
#5524=CARTESIAN_POINT('',(-19.,-20.,0.));
#5525=CARTESIAN_POINT('Origin',(-20.,20.,0.));
#5526=CARTESIAN_POINT('',(-20.,19.,720.));
#5527=CARTESIAN_POINT('',(-20.,20.,720.));
#5528=CARTESIAN_POINT('',(-20.,19.,0.));
#5529=CARTESIAN_POINT('',(-20.,19.,0.));
#5530=CARTESIAN_POINT('',(-20.,20.,0.));
#5531=CARTESIAN_POINT('Origin',(0.,0.,720.));
#5532=CARTESIAN_POINT('',(19.,-20.,720.));
#5533=CARTESIAN_POINT('',(-20.,-20.,720.));
#5534=CARTESIAN_POINT('',(20.,-19.,720.));
#5535=CARTESIAN_POINT('Origin',(19.,-19.,720.));
#5536=CARTESIAN_POINT('',(20.,19.,720.));
#5537=CARTESIAN_POINT('',(20.,-20.,720.));
#5538=CARTESIAN_POINT('',(19.,20.,720.));
#5539=CARTESIAN_POINT('Origin',(19.,19.,720.));
#5540=CARTESIAN_POINT('',(-19.,20.,720.));
#5541=CARTESIAN_POINT('',(20.,20.,720.));
#5542=CARTESIAN_POINT('Origin',(-19.,19.,720.));
#5543=CARTESIAN_POINT('',(-16.,-15.,720.));
#5544=CARTESIAN_POINT('',(-16.,15.,720.));
#5545=CARTESIAN_POINT('',(-16.,16.,720.));
#5546=CARTESIAN_POINT('',(-15.,16.,720.));
#5547=CARTESIAN_POINT('Origin',(-15.,15.,720.));
#5548=CARTESIAN_POINT('',(15.,16.,720.));
#5549=CARTESIAN_POINT('',(16.,16.,720.));
#5550=CARTESIAN_POINT('',(16.,15.,720.));
#5551=CARTESIAN_POINT('Origin',(15.,15.,720.));
#5552=CARTESIAN_POINT('',(16.,-15.,720.));
#5553=CARTESIAN_POINT('',(16.,-16.,720.));
#5554=CARTESIAN_POINT('',(15.,-16.,720.));
#5555=CARTESIAN_POINT('Origin',(15.,-15.,720.));
#5556=CARTESIAN_POINT('',(-15.,-16.,720.));
#5557=CARTESIAN_POINT('',(-16.,-16.,720.));
#5558=CARTESIAN_POINT('Origin',(-15.,-15.,720.));
#5559=CARTESIAN_POINT('Origin',(19.,-19.,0.));
#5560=CARTESIAN_POINT('',(19.,-20.,0.));
#5561=CARTESIAN_POINT('',(19.,-20.,0.));
#5562=CARTESIAN_POINT('',(20.,-19.,0.));
#5563=CARTESIAN_POINT('Origin',(19.,-19.,0.));
#5564=CARTESIAN_POINT('',(20.,-19.,0.));
#5565=CARTESIAN_POINT('Origin',(20.,-20.,0.));
#5566=CARTESIAN_POINT('',(20.,19.,0.));
#5567=CARTESIAN_POINT('',(20.,-20.,0.));
#5568=CARTESIAN_POINT('',(20.,19.,0.));
#5569=CARTESIAN_POINT('Origin',(19.,19.,0.));
#5570=CARTESIAN_POINT('',(19.,20.,0.));
#5571=CARTESIAN_POINT('Origin',(19.,19.,0.));
#5572=CARTESIAN_POINT('',(19.,20.,0.));
#5573=CARTESIAN_POINT('Origin',(-19.,19.,0.));
#5574=CARTESIAN_POINT('',(-19.,20.,0.));
#5575=CARTESIAN_POINT('',(-19.,20.,0.));
#5576=CARTESIAN_POINT('Origin',(-19.,19.,0.));
#5577=CARTESIAN_POINT('Origin',(-15.,15.,0.));
#5578=CARTESIAN_POINT('',(-16.,15.,0.));
#5579=CARTESIAN_POINT('',(-15.,16.,0.));
#5580=CARTESIAN_POINT('Origin',(-15.,15.,0.));
#5581=CARTESIAN_POINT('',(-15.,16.,0.));
#5582=CARTESIAN_POINT('',(-16.,15.,0.));
#5583=CARTESIAN_POINT('Origin',(-16.,16.,0.));
#5584=CARTESIAN_POINT('',(15.,16.,0.));
#5585=CARTESIAN_POINT('',(16.,16.,0.));
#5586=CARTESIAN_POINT('',(15.,16.,0.));
#5587=CARTESIAN_POINT('Origin',(15.,15.,0.));
#5588=CARTESIAN_POINT('',(16.,15.,0.));
#5589=CARTESIAN_POINT('Origin',(15.,15.,0.));
#5590=CARTESIAN_POINT('',(16.,15.,0.));
#5591=CARTESIAN_POINT('Origin',(16.,16.,0.));
#5592=CARTESIAN_POINT('',(16.,-15.,0.));
#5593=CARTESIAN_POINT('',(16.,-16.,0.));
#5594=CARTESIAN_POINT('',(16.,-15.,0.));
#5595=CARTESIAN_POINT('Origin',(15.,-15.,0.));
#5596=CARTESIAN_POINT('',(15.,-16.,0.));
#5597=CARTESIAN_POINT('Origin',(15.,-15.,0.));
#5598=CARTESIAN_POINT('',(15.,-16.,0.));
#5599=CARTESIAN_POINT('Origin',(16.,-16.,0.));
#5600=CARTESIAN_POINT('',(-15.,-16.,0.));
#5601=CARTESIAN_POINT('',(-16.,-16.,0.));
#5602=CARTESIAN_POINT('',(-15.,-16.,0.));
#5603=CARTESIAN_POINT('Origin',(-15.,-15.,0.));
#5604=CARTESIAN_POINT('',(-16.,-15.,0.));
#5605=CARTESIAN_POINT('Origin',(-15.,-15.,0.));
#5606=CARTESIAN_POINT('',(-16.,-15.,0.));
#5607=CARTESIAN_POINT('Origin',(-16.,-16.,0.));
#5608=CARTESIAN_POINT('',(-16.,16.,0.));
#5609=CARTESIAN_POINT('Origin',(20.,20.,0.));
#5610=CARTESIAN_POINT('',(20.,20.,0.));
#5611=CARTESIAN_POINT('Origin',(-20.,-20.,0.));
#5612=CARTESIAN_POINT('',(-20.,-20.,0.));
#5613=CARTESIAN_POINT('Origin',(0.,0.,0.));
#5614=CARTESIAN_POINT('',(0.,0.,0.));
#5615=CARTESIAN_POINT('Origin',(-19.,-19.,0.));
#5616=CARTESIAN_POINT('',(-19.,-20.,520.));
#5617=CARTESIAN_POINT('',(-20.,-19.,520.));
#5618=CARTESIAN_POINT('Origin',(-19.,-19.,520.));
#5619=CARTESIAN_POINT('',(-20.,-19.,0.));
#5620=CARTESIAN_POINT('',(-20.,-19.,0.));
#5621=CARTESIAN_POINT('',(-19.,-20.,0.));
#5622=CARTESIAN_POINT('Origin',(-19.,-19.,0.));
#5623=CARTESIAN_POINT('',(-19.,-20.,0.));
#5624=CARTESIAN_POINT('Origin',(-20.,20.,0.));
#5625=CARTESIAN_POINT('',(-20.,19.,520.));
#5626=CARTESIAN_POINT('',(-20.,20.,520.));
#5627=CARTESIAN_POINT('',(-20.,19.,0.));
#5628=CARTESIAN_POINT('',(-20.,19.,0.));
#5629=CARTESIAN_POINT('',(-20.,20.,0.));
#5630=CARTESIAN_POINT('Origin',(0.,0.,520.));
#5631=CARTESIAN_POINT('',(19.,-20.,520.));
#5632=CARTESIAN_POINT('',(-20.,-20.,520.));
#5633=CARTESIAN_POINT('',(20.,-19.,520.));
#5634=CARTESIAN_POINT('Origin',(19.,-19.,520.));
#5635=CARTESIAN_POINT('',(20.,19.,520.));
#5636=CARTESIAN_POINT('',(20.,-20.,520.));
#5637=CARTESIAN_POINT('',(19.,20.,520.));
#5638=CARTESIAN_POINT('Origin',(19.,19.,520.));
#5639=CARTESIAN_POINT('',(-19.,20.,520.));
#5640=CARTESIAN_POINT('',(20.,20.,520.));
#5641=CARTESIAN_POINT('Origin',(-19.,19.,520.));
#5642=CARTESIAN_POINT('',(-16.,-15.,520.));
#5643=CARTESIAN_POINT('',(-16.,15.,520.));
#5644=CARTESIAN_POINT('',(-16.,16.,520.));
#5645=CARTESIAN_POINT('',(-15.,16.,520.));
#5646=CARTESIAN_POINT('Origin',(-15.,15.,520.));
#5647=CARTESIAN_POINT('',(15.,16.,520.));
#5648=CARTESIAN_POINT('',(16.,16.,520.));
#5649=CARTESIAN_POINT('',(16.,15.,520.));
#5650=CARTESIAN_POINT('Origin',(15.,15.,520.));
#5651=CARTESIAN_POINT('',(16.,-15.,520.));
#5652=CARTESIAN_POINT('',(16.,-16.,520.));
#5653=CARTESIAN_POINT('',(15.,-16.,520.));
#5654=CARTESIAN_POINT('Origin',(15.,-15.,520.));
#5655=CARTESIAN_POINT('',(-15.,-16.,520.));
#5656=CARTESIAN_POINT('',(-16.,-16.,520.));
#5657=CARTESIAN_POINT('Origin',(-15.,-15.,520.));
#5658=CARTESIAN_POINT('Origin',(19.,-19.,0.));
#5659=CARTESIAN_POINT('',(19.,-20.,0.));
#5660=CARTESIAN_POINT('',(19.,-20.,0.));
#5661=CARTESIAN_POINT('',(20.,-19.,0.));
#5662=CARTESIAN_POINT('Origin',(19.,-19.,0.));
#5663=CARTESIAN_POINT('',(20.,-19.,0.));
#5664=CARTESIAN_POINT('Origin',(20.,-20.,0.));
#5665=CARTESIAN_POINT('',(20.,19.,0.));
#5666=CARTESIAN_POINT('',(20.,-20.,0.));
#5667=CARTESIAN_POINT('',(20.,19.,0.));
#5668=CARTESIAN_POINT('Origin',(19.,19.,0.));
#5669=CARTESIAN_POINT('',(19.,20.,0.));
#5670=CARTESIAN_POINT('Origin',(19.,19.,0.));
#5671=CARTESIAN_POINT('',(19.,20.,0.));
#5672=CARTESIAN_POINT('Origin',(-19.,19.,0.));
#5673=CARTESIAN_POINT('',(-19.,20.,0.));
#5674=CARTESIAN_POINT('',(-19.,20.,0.));
#5675=CARTESIAN_POINT('Origin',(-19.,19.,0.));
#5676=CARTESIAN_POINT('Origin',(-15.,15.,0.));
#5677=CARTESIAN_POINT('',(-16.,15.,0.));
#5678=CARTESIAN_POINT('',(-15.,16.,0.));
#5679=CARTESIAN_POINT('Origin',(-15.,15.,0.));
#5680=CARTESIAN_POINT('',(-15.,16.,0.));
#5681=CARTESIAN_POINT('',(-16.,15.,0.));
#5682=CARTESIAN_POINT('Origin',(-16.,16.,0.));
#5683=CARTESIAN_POINT('',(15.,16.,0.));
#5684=CARTESIAN_POINT('',(16.,16.,0.));
#5685=CARTESIAN_POINT('',(15.,16.,0.));
#5686=CARTESIAN_POINT('Origin',(15.,15.,0.));
#5687=CARTESIAN_POINT('',(16.,15.,0.));
#5688=CARTESIAN_POINT('Origin',(15.,15.,0.));
#5689=CARTESIAN_POINT('',(16.,15.,0.));
#5690=CARTESIAN_POINT('Origin',(16.,16.,0.));
#5691=CARTESIAN_POINT('',(16.,-15.,0.));
#5692=CARTESIAN_POINT('',(16.,-16.,0.));
#5693=CARTESIAN_POINT('',(16.,-15.,0.));
#5694=CARTESIAN_POINT('Origin',(15.,-15.,0.));
#5695=CARTESIAN_POINT('',(15.,-16.,0.));
#5696=CARTESIAN_POINT('Origin',(15.,-15.,0.));
#5697=CARTESIAN_POINT('',(15.,-16.,0.));
#5698=CARTESIAN_POINT('Origin',(16.,-16.,0.));
#5699=CARTESIAN_POINT('',(-15.,-16.,0.));
#5700=CARTESIAN_POINT('',(-16.,-16.,0.));
#5701=CARTESIAN_POINT('',(-15.,-16.,0.));
#5702=CARTESIAN_POINT('Origin',(-15.,-15.,0.));
#5703=CARTESIAN_POINT('',(-16.,-15.,0.));
#5704=CARTESIAN_POINT('Origin',(-15.,-15.,0.));
#5705=CARTESIAN_POINT('',(-16.,-15.,0.));
#5706=CARTESIAN_POINT('Origin',(-16.,-16.,0.));
#5707=CARTESIAN_POINT('',(-16.,16.,0.));
#5708=CARTESIAN_POINT('Origin',(20.,20.,0.));
#5709=CARTESIAN_POINT('',(20.,20.,0.));
#5710=CARTESIAN_POINT('Origin',(-20.,-20.,0.));
#5711=CARTESIAN_POINT('',(-20.,-20.,0.));
#5712=CARTESIAN_POINT('Origin',(0.,0.,0.));
#5713=CARTESIAN_POINT('',(0.,0.,0.));
#5714=CARTESIAN_POINT('Origin',(30.,3.,60.));
#5715=CARTESIAN_POINT('',(30.,6.,55.5));
#5716=CARTESIAN_POINT('Origin',(30.,6.,60.));
#5717=CARTESIAN_POINT('',(30.,0.,55.5));
#5718=CARTESIAN_POINT('',(30.,3.,55.5));
#5719=CARTESIAN_POINT('Origin',(30.,0.,60.));
#5720=CARTESIAN_POINT('Origin',(30.,3.,660.));
#5721=CARTESIAN_POINT('',(30.,6.,655.5));
#5722=CARTESIAN_POINT('Origin',(30.,6.,660.));
#5723=CARTESIAN_POINT('',(30.,0.,655.5));
#5724=CARTESIAN_POINT('',(30.,3.,655.5));
#5725=CARTESIAN_POINT('Origin',(30.,0.,660.));
#5726=CARTESIAN_POINT('Origin',(1.,1.,0.));
#5727=CARTESIAN_POINT('',(1.,0.,720.));
#5728=CARTESIAN_POINT('',(0.,1.,720.));
#5729=CARTESIAN_POINT('Origin',(1.,1.,720.));
#5730=CARTESIAN_POINT('',(0.,1.,0.));
#5731=CARTESIAN_POINT('',(0.,1.,0.));
#5732=CARTESIAN_POINT('',(1.,0.,0.));
#5733=CARTESIAN_POINT('Origin',(1.,1.,0.));
#5734=CARTESIAN_POINT('',(1.,0.,0.));
#5735=CARTESIAN_POINT('Origin',(30.,20.,720.));
#5736=CARTESIAN_POINT('',(59.,0.,720.));
#5737=CARTESIAN_POINT('',(0.,0.,720.));
#5738=CARTESIAN_POINT('',(60.,1.,720.));
#5739=CARTESIAN_POINT('Origin',(59.,1.,720.));
#5740=CARTESIAN_POINT('',(60.,39.,720.));
#5741=CARTESIAN_POINT('',(60.,0.,720.));
#5742=CARTESIAN_POINT('',(59.,40.,720.));
#5743=CARTESIAN_POINT('Origin',(59.,39.,720.));
#5744=CARTESIAN_POINT('',(55.,40.,720.));
#5745=CARTESIAN_POINT('',(60.,40.,720.));
#5746=CARTESIAN_POINT('',(54.,39.,720.));
#5747=CARTESIAN_POINT('Origin',(55.,39.,720.));
#5748=CARTESIAN_POINT('',(54.,7.,720.));
#5749=CARTESIAN_POINT('',(54.,40.,720.));
#5750=CARTESIAN_POINT('',(53.,6.,720.));
#5751=CARTESIAN_POINT('Origin',(53.,7.,720.));
#5752=CARTESIAN_POINT('',(6.99999999999999,6.,720.));
#5753=CARTESIAN_POINT('',(54.,6.,720.));
#5754=CARTESIAN_POINT('',(6.,7.,720.));
#5755=CARTESIAN_POINT('Origin',(7.,7.,720.));
#5756=CARTESIAN_POINT('',(6.,39.,720.));
#5757=CARTESIAN_POINT('',(6.,6.,720.));
#5758=CARTESIAN_POINT('',(5.,40.,720.));
#5759=CARTESIAN_POINT('Origin',(5.,39.,720.));
#5760=CARTESIAN_POINT('',(1.,40.,720.));
#5761=CARTESIAN_POINT('',(6.,40.,720.));
#5762=CARTESIAN_POINT('',(0.,39.,720.));
#5763=CARTESIAN_POINT('Origin',(1.,39.,720.));
#5764=CARTESIAN_POINT('',(0.,40.,720.));
#5765=CARTESIAN_POINT('Origin',(0.,0.,0.));
#5766=CARTESIAN_POINT('',(59.,0.,0.));
#5767=CARTESIAN_POINT('',(0.,0.,0.));
#5768=CARTESIAN_POINT('',(59.,0.,0.));
#5769=CARTESIAN_POINT('Origin',(59.,1.,0.));
#5770=CARTESIAN_POINT('',(60.,1.,0.));
#5771=CARTESIAN_POINT('Origin',(59.,1.,0.));
#5772=CARTESIAN_POINT('',(60.,1.,0.));
#5773=CARTESIAN_POINT('Origin',(59.,39.,0.));
#5774=CARTESIAN_POINT('',(60.,39.,0.));
#5775=CARTESIAN_POINT('',(60.,39.,0.));
#5776=CARTESIAN_POINT('',(59.,40.,0.));
#5777=CARTESIAN_POINT('Origin',(59.,39.,0.));
#5778=CARTESIAN_POINT('',(59.,40.,0.));
#5779=CARTESIAN_POINT('Origin',(60.,40.,0.));
#5780=CARTESIAN_POINT('',(55.,40.,0.));
#5781=CARTESIAN_POINT('',(60.,40.,0.));
#5782=CARTESIAN_POINT('',(55.,40.,0.));
#5783=CARTESIAN_POINT('Origin',(55.,39.,0.));
#5784=CARTESIAN_POINT('',(54.,39.,0.));
#5785=CARTESIAN_POINT('Origin',(55.,39.,0.));
#5786=CARTESIAN_POINT('',(54.,39.,0.));
#5787=CARTESIAN_POINT('Origin',(53.,7.,0.));
#5788=CARTESIAN_POINT('',(54.,7.,0.));
#5789=CARTESIAN_POINT('',(53.,6.,0.));
#5790=CARTESIAN_POINT('Origin',(53.,7.,0.));
#5791=CARTESIAN_POINT('',(53.,6.,0.));
#5792=CARTESIAN_POINT('',(54.,7.,0.));
#5793=CARTESIAN_POINT('Origin',(54.,6.,0.));
#5794=CARTESIAN_POINT('',(6.99999999999999,6.,0.));
#5795=CARTESIAN_POINT('',(54.,6.,0.));
#5796=CARTESIAN_POINT('',(7.,6.,0.));
#5797=CARTESIAN_POINT('Origin',(7.,7.,0.));
#5798=CARTESIAN_POINT('',(6.,7.,0.));
#5799=CARTESIAN_POINT('Origin',(7.,7.,0.));
#5800=CARTESIAN_POINT('',(6.,7.,0.));
#5801=CARTESIAN_POINT('Origin',(6.,6.,0.));
#5802=CARTESIAN_POINT('',(6.,39.,0.));
#5803=CARTESIAN_POINT('',(6.,6.,0.));
#5804=CARTESIAN_POINT('',(6.,39.,0.));
#5805=CARTESIAN_POINT('Origin',(5.,39.,0.));
#5806=CARTESIAN_POINT('',(5.,40.,0.));
#5807=CARTESIAN_POINT('Origin',(5.,39.,0.));
#5808=CARTESIAN_POINT('',(5.,40.,0.));
#5809=CARTESIAN_POINT('Origin',(1.,39.,0.));
#5810=CARTESIAN_POINT('',(1.,40.,0.));
#5811=CARTESIAN_POINT('',(1.,40.,0.));
#5812=CARTESIAN_POINT('',(0.,39.,0.));
#5813=CARTESIAN_POINT('Origin',(1.,39.,0.));
#5814=CARTESIAN_POINT('',(0.,39.,0.));
#5815=CARTESIAN_POINT('Origin',(0.,40.,0.));
#5816=CARTESIAN_POINT('',(0.,40.,0.));
#5817=CARTESIAN_POINT('Origin',(6.,40.,0.));
#5818=CARTESIAN_POINT('',(6.,40.,0.));
#5819=CARTESIAN_POINT('Origin',(54.,40.,0.));
#5820=CARTESIAN_POINT('',(54.,40.,0.));
#5821=CARTESIAN_POINT('Origin',(60.,0.,0.));
#5822=CARTESIAN_POINT('',(60.,0.,0.));
#5823=CARTESIAN_POINT('Origin',(30.,20.,0.));
#5824=CARTESIAN_POINT('',(0.,0.,0.));
#5825=CARTESIAN_POINT('Origin',(300.,180.,2.));
#5826=CARTESIAN_POINT('',(296.5,180.,4.));
#5827=CARTESIAN_POINT('Origin',(300.,180.,4.));
#5828=CARTESIAN_POINT('',(296.5,180.,0.));
#5829=CARTESIAN_POINT('',(296.5,180.,2.));
#5830=CARTESIAN_POINT('Origin',(300.,180.,0.));
#5831=CARTESIAN_POINT('Origin',(300.,-280.,2.));
#5832=CARTESIAN_POINT('',(296.5,-280.,4.));
#5833=CARTESIAN_POINT('Origin',(300.,-280.,4.));
#5834=CARTESIAN_POINT('',(296.5,-280.,0.));
#5835=CARTESIAN_POINT('',(296.5,-280.,2.));
#5836=CARTESIAN_POINT('Origin',(300.,-280.,0.));
#5837=CARTESIAN_POINT('Origin',(-300.,180.,2.));
#5838=CARTESIAN_POINT('',(-303.5,180.,4.));
#5839=CARTESIAN_POINT('Origin',(-300.,180.,4.));
#5840=CARTESIAN_POINT('',(-303.5,180.,0.));
#5841=CARTESIAN_POINT('',(-303.5,180.,2.));
#5842=CARTESIAN_POINT('Origin',(-300.,180.,0.));
#5843=CARTESIAN_POINT('Origin',(-300.,-280.,2.));
#5844=CARTESIAN_POINT('',(-303.5,-280.,4.));
#5845=CARTESIAN_POINT('Origin',(-300.,-280.,4.));
#5846=CARTESIAN_POINT('',(-303.5,-280.,0.));
#5847=CARTESIAN_POINT('',(-303.5,-280.,2.));
#5848=CARTESIAN_POINT('Origin',(-300.,-280.,0.));
#5849=CARTESIAN_POINT('Origin',(-300.,-180.,2.));
#5850=CARTESIAN_POINT('',(-303.5,-180.,4.));
#5851=CARTESIAN_POINT('Origin',(-300.,-180.,4.));
#5852=CARTESIAN_POINT('',(-303.5,-180.,0.));
#5853=CARTESIAN_POINT('',(-303.5,-180.,2.));
#5854=CARTESIAN_POINT('Origin',(-300.,-180.,0.));
#5855=CARTESIAN_POINT('Origin',(-300.,280.,2.));
#5856=CARTESIAN_POINT('',(-303.5,280.,4.));
#5857=CARTESIAN_POINT('Origin',(-300.,280.,4.));
#5858=CARTESIAN_POINT('',(-303.5,280.,0.));
#5859=CARTESIAN_POINT('',(-303.5,280.,2.));
#5860=CARTESIAN_POINT('Origin',(-300.,280.,0.));
#5861=CARTESIAN_POINT('Origin',(300.,-180.,2.));
#5862=CARTESIAN_POINT('',(296.5,-180.,4.));
#5863=CARTESIAN_POINT('Origin',(300.,-180.,4.));
#5864=CARTESIAN_POINT('',(296.5,-180.,0.));
#5865=CARTESIAN_POINT('',(296.5,-180.,2.));
#5866=CARTESIAN_POINT('Origin',(300.,-180.,0.));
#5867=CARTESIAN_POINT('Origin',(300.,280.,2.));
#5868=CARTESIAN_POINT('',(296.5,280.,4.));
#5869=CARTESIAN_POINT('Origin',(300.,280.,4.));
#5870=CARTESIAN_POINT('',(296.5,280.,0.));
#5871=CARTESIAN_POINT('',(296.5,280.,2.));
#5872=CARTESIAN_POINT('Origin',(300.,280.,0.));
#5873=CARTESIAN_POINT('Origin',(360.,-260.,4.));
#5874=CARTESIAN_POINT('',(360.,-260.,4.));
#5875=CARTESIAN_POINT('',(380.,-260.,4.));
#5876=CARTESIAN_POINT('',(180.,-260.,4.));
#5877=CARTESIAN_POINT('',(360.,-260.,0.));
#5878=CARTESIAN_POINT('',(360.,-260.,4.));
#5879=CARTESIAN_POINT('',(380.,-260.,0.));
#5880=CARTESIAN_POINT('',(180.,-260.,0.));
#5881=CARTESIAN_POINT('',(380.,-260.,2.));
#5882=CARTESIAN_POINT('Origin',(360.,-300.,4.));
#5883=CARTESIAN_POINT('',(360.,-300.,4.));
#5884=CARTESIAN_POINT('',(360.,-150.,4.));
#5885=CARTESIAN_POINT('',(360.,-300.,0.));
#5886=CARTESIAN_POINT('',(360.,-300.,2.));
#5887=CARTESIAN_POINT('',(360.,-150.,0.));
#5888=CARTESIAN_POINT('Origin',(-360.,260.,4.));
#5889=CARTESIAN_POINT('',(-360.,260.,4.));
#5890=CARTESIAN_POINT('',(-380.,260.,4.));
#5891=CARTESIAN_POINT('',(-180.,260.,4.));
#5892=CARTESIAN_POINT('',(-360.,260.,0.));
#5893=CARTESIAN_POINT('',(-360.,260.,4.));
#5894=CARTESIAN_POINT('',(-380.,260.,0.));
#5895=CARTESIAN_POINT('',(-180.,260.,0.));
#5896=CARTESIAN_POINT('',(-380.,260.,2.));
#5897=CARTESIAN_POINT('Origin',(-360.,300.,4.));
#5898=CARTESIAN_POINT('',(-360.,300.,4.));
#5899=CARTESIAN_POINT('',(-360.,150.,4.));
#5900=CARTESIAN_POINT('',(-360.,300.,0.));
#5901=CARTESIAN_POINT('',(-360.,300.,2.));
#5902=CARTESIAN_POINT('',(-360.,150.,0.));
#5903=CARTESIAN_POINT('Origin',(-360.,-260.,4.));
#5904=CARTESIAN_POINT('',(-360.,-260.,4.));
#5905=CARTESIAN_POINT('',(-360.,-300.,4.));
#5906=CARTESIAN_POINT('',(-360.,-130.,4.));
#5907=CARTESIAN_POINT('',(-360.,-260.,0.));
#5908=CARTESIAN_POINT('',(-360.,-260.,4.));
#5909=CARTESIAN_POINT('',(-360.,-300.,0.));
#5910=CARTESIAN_POINT('',(-360.,-130.,0.));
#5911=CARTESIAN_POINT('',(-360.,-300.,2.));
#5912=CARTESIAN_POINT('Origin',(-380.,-260.,4.));
#5913=CARTESIAN_POINT('',(-380.,-260.,4.));
#5914=CARTESIAN_POINT('',(-190.,-260.,4.));
#5915=CARTESIAN_POINT('',(-380.,-260.,0.));
#5916=CARTESIAN_POINT('',(-380.,-260.,2.));
#5917=CARTESIAN_POINT('',(-190.,-260.,0.));
#5918=CARTESIAN_POINT('Origin',(380.,260.,4.));
#5919=CARTESIAN_POINT('',(380.,260.,4.));
#5920=CARTESIAN_POINT('',(360.,260.,4.));
#5921=CARTESIAN_POINT('',(190.,260.,4.));
#5922=CARTESIAN_POINT('',(380.,260.,0.));
#5923=CARTESIAN_POINT('',(380.,260.,2.));
#5924=CARTESIAN_POINT('',(360.,260.,0.));
#5925=CARTESIAN_POINT('',(190.,260.,0.));
#5926=CARTESIAN_POINT('',(360.,260.,4.));
#5927=CARTESIAN_POINT('Origin',(360.,260.,4.));
#5928=CARTESIAN_POINT('',(360.,300.,4.));
#5929=CARTESIAN_POINT('',(360.,130.,4.));
#5930=CARTESIAN_POINT('',(360.,300.,0.));
#5931=CARTESIAN_POINT('',(360.,130.,0.));
#5932=CARTESIAN_POINT('',(360.,300.,2.));
#5933=CARTESIAN_POINT('Origin',(-380.,300.,0.));
#5934=CARTESIAN_POINT('',(-380.,300.,0.));
#5935=CARTESIAN_POINT('',(-380.,300.,4.));
#5936=CARTESIAN_POINT('Origin',(380.,300.,0.));
#5937=CARTESIAN_POINT('',(380.,300.,4.));
#5938=CARTESIAN_POINT('',(380.,300.,0.));
#5939=CARTESIAN_POINT('Origin',(0.,0.,0.));
#5940=CARTESIAN_POINT('',(-380.,-300.,0.));
#5941=CARTESIAN_POINT('',(380.,-300.,0.));
#5942=CARTESIAN_POINT('Origin',(0.,0.,4.));
#5943=CARTESIAN_POINT('',(380.,-300.,4.));
#5944=CARTESIAN_POINT('',(-380.,-300.,4.));
#5945=CARTESIAN_POINT('Origin',(380.,-300.,0.));
#5946=CARTESIAN_POINT('Origin',(-380.,-300.,0.));
#5947=CARTESIAN_POINT('',(0.,0.,0.));
#5948=CARTESIAN_POINT('Origin',(40.,-40.,5.));
#5949=CARTESIAN_POINT('',(33.,-40.,10.));
#5950=CARTESIAN_POINT('Origin',(40.,-40.,10.));
#5951=CARTESIAN_POINT('',(33.,-40.,0.));
#5952=CARTESIAN_POINT('',(33.,-40.,5.));
#5953=CARTESIAN_POINT('Origin',(40.,-40.,0.));
#5954=CARTESIAN_POINT('Origin',(-40.,-40.,5.));
#5955=CARTESIAN_POINT('',(-47.,-40.,10.));
#5956=CARTESIAN_POINT('Origin',(-40.,-40.,10.));
#5957=CARTESIAN_POINT('',(-47.,-40.,0.));
#5958=CARTESIAN_POINT('',(-47.,-40.,5.));
#5959=CARTESIAN_POINT('Origin',(-40.,-40.,0.));
#5960=CARTESIAN_POINT('Origin',(-40.,40.,5.));
#5961=CARTESIAN_POINT('',(-47.,40.,10.));
#5962=CARTESIAN_POINT('Origin',(-40.,40.,10.));
#5963=CARTESIAN_POINT('',(-47.,40.,0.));
#5964=CARTESIAN_POINT('',(-47.,40.,5.));
#5965=CARTESIAN_POINT('Origin',(-40.,40.,0.));
#5966=CARTESIAN_POINT('Origin',(40.,40.,5.));
#5967=CARTESIAN_POINT('',(33.,40.,10.));
#5968=CARTESIAN_POINT('Origin',(40.,40.,10.));
#5969=CARTESIAN_POINT('',(33.,40.,0.));
#5970=CARTESIAN_POINT('',(33.,40.,5.));
#5971=CARTESIAN_POINT('Origin',(40.,40.,0.));
#5972=CARTESIAN_POINT('Origin',(50.,50.,0.));
#5973=CARTESIAN_POINT('',(50.,50.,0.));
#5974=CARTESIAN_POINT('',(-50.,50.,0.));
#5975=CARTESIAN_POINT('',(50.,50.,0.));
#5976=CARTESIAN_POINT('',(-50.,50.,10.));
#5977=CARTESIAN_POINT('',(-50.,50.,0.));
#5978=CARTESIAN_POINT('',(50.,50.,10.));
#5979=CARTESIAN_POINT('',(50.,50.,10.));
#5980=CARTESIAN_POINT('',(50.,50.,0.));
#5981=CARTESIAN_POINT('Origin',(50.,-50.,0.));
#5982=CARTESIAN_POINT('',(50.,-50.,0.));
#5983=CARTESIAN_POINT('',(50.,-50.,0.));
#5984=CARTESIAN_POINT('',(50.,-50.,10.));
#5985=CARTESIAN_POINT('',(50.,-50.,10.));
#5986=CARTESIAN_POINT('',(50.,-50.,0.));
#5987=CARTESIAN_POINT('Origin',(-50.,-50.,0.));
#5988=CARTESIAN_POINT('',(-50.,-50.,0.));
#5989=CARTESIAN_POINT('',(-50.,-50.,0.));
#5990=CARTESIAN_POINT('',(-50.,-50.,10.));
#5991=CARTESIAN_POINT('',(-50.,-50.,10.));
#5992=CARTESIAN_POINT('',(-50.,-50.,0.));
#5993=CARTESIAN_POINT('Origin',(-50.,50.,0.));
#5994=CARTESIAN_POINT('',(-50.,50.,0.));
#5995=CARTESIAN_POINT('',(-50.,50.,10.));
#5996=CARTESIAN_POINT('Origin',(0.,0.,10.));
#5997=CARTESIAN_POINT('Origin',(0.,0.,0.));
#5998=CARTESIAN_POINT('',(0.,0.,0.));
#5999=CARTESIAN_POINT('Origin',(40.,-40.,5.));
#6000=CARTESIAN_POINT('',(33.,-40.,10.));
#6001=CARTESIAN_POINT('Origin',(40.,-40.,10.));
#6002=CARTESIAN_POINT('',(33.,-40.,0.));
#6003=CARTESIAN_POINT('',(33.,-40.,5.));
#6004=CARTESIAN_POINT('Origin',(40.,-40.,0.));
#6005=CARTESIAN_POINT('Origin',(-40.,-40.,5.));
#6006=CARTESIAN_POINT('',(-47.,-40.,10.));
#6007=CARTESIAN_POINT('Origin',(-40.,-40.,10.));
#6008=CARTESIAN_POINT('',(-47.,-40.,0.));
#6009=CARTESIAN_POINT('',(-47.,-40.,5.));
#6010=CARTESIAN_POINT('Origin',(-40.,-40.,0.));
#6011=CARTESIAN_POINT('Origin',(-40.,40.,5.));
#6012=CARTESIAN_POINT('',(-47.,40.,10.));
#6013=CARTESIAN_POINT('Origin',(-40.,40.,10.));
#6014=CARTESIAN_POINT('',(-47.,40.,0.));
#6015=CARTESIAN_POINT('',(-47.,40.,5.));
#6016=CARTESIAN_POINT('Origin',(-40.,40.,0.));
#6017=CARTESIAN_POINT('Origin',(40.,40.,5.));
#6018=CARTESIAN_POINT('',(33.,40.,10.));
#6019=CARTESIAN_POINT('Origin',(40.,40.,10.));
#6020=CARTESIAN_POINT('',(33.,40.,0.));
#6021=CARTESIAN_POINT('',(33.,40.,5.));
#6022=CARTESIAN_POINT('Origin',(40.,40.,0.));
#6023=CARTESIAN_POINT('Origin',(50.,50.,0.));
#6024=CARTESIAN_POINT('',(50.,50.,0.));
#6025=CARTESIAN_POINT('',(-50.,50.,0.));
#6026=CARTESIAN_POINT('',(50.,50.,0.));
#6027=CARTESIAN_POINT('',(-50.,50.,10.));
#6028=CARTESIAN_POINT('',(-50.,50.,0.));
#6029=CARTESIAN_POINT('',(50.,50.,10.));
#6030=CARTESIAN_POINT('',(50.,50.,10.));
#6031=CARTESIAN_POINT('',(50.,50.,0.));
#6032=CARTESIAN_POINT('Origin',(50.,-50.,0.));
#6033=CARTESIAN_POINT('',(50.,-50.,0.));
#6034=CARTESIAN_POINT('',(50.,-50.,0.));
#6035=CARTESIAN_POINT('',(50.,-50.,10.));
#6036=CARTESIAN_POINT('',(50.,-50.,10.));
#6037=CARTESIAN_POINT('',(50.,-50.,0.));
#6038=CARTESIAN_POINT('Origin',(-50.,-50.,0.));
#6039=CARTESIAN_POINT('',(-50.,-50.,0.));
#6040=CARTESIAN_POINT('',(-50.,-50.,0.));
#6041=CARTESIAN_POINT('',(-50.,-50.,10.));
#6042=CARTESIAN_POINT('',(-50.,-50.,10.));
#6043=CARTESIAN_POINT('',(-50.,-50.,0.));
#6044=CARTESIAN_POINT('Origin',(-50.,50.,0.));
#6045=CARTESIAN_POINT('',(-50.,50.,0.));
#6046=CARTESIAN_POINT('',(-50.,50.,10.));
#6047=CARTESIAN_POINT('Origin',(0.,0.,10.));
#6048=CARTESIAN_POINT('Origin',(0.,0.,0.));
#6049=CARTESIAN_POINT('',(0.,0.,0.));
#6050=CARTESIAN_POINT('Origin',(20.,20.,0.));
#6051=CARTESIAN_POINT('',(20.,20.,0.));
#6052=CARTESIAN_POINT('',(-20.,20.,0.));
#6053=CARTESIAN_POINT('',(20.,20.,0.));
#6054=CARTESIAN_POINT('',(-20.,20.,4.));
#6055=CARTESIAN_POINT('',(-20.,20.,0.));
#6056=CARTESIAN_POINT('',(20.,20.,4.));
#6057=CARTESIAN_POINT('',(20.,20.,4.));
#6058=CARTESIAN_POINT('',(20.,20.,0.));
#6059=CARTESIAN_POINT('Origin',(20.,-20.,0.));
#6060=CARTESIAN_POINT('',(20.,-20.,0.));
#6061=CARTESIAN_POINT('',(20.,-20.,0.));
#6062=CARTESIAN_POINT('',(20.,-20.,4.));
#6063=CARTESIAN_POINT('',(20.,-20.,4.));
#6064=CARTESIAN_POINT('',(20.,-20.,0.));
#6065=CARTESIAN_POINT('Origin',(-20.,-20.,0.));
#6066=CARTESIAN_POINT('',(-20.,-20.,0.));
#6067=CARTESIAN_POINT('',(-20.,-20.,0.));
#6068=CARTESIAN_POINT('',(-20.,-20.,4.));
#6069=CARTESIAN_POINT('',(-20.,-20.,4.));
#6070=CARTESIAN_POINT('',(-20.,-20.,0.));
#6071=CARTESIAN_POINT('Origin',(-20.,20.,0.));
#6072=CARTESIAN_POINT('',(-20.,20.,0.));
#6073=CARTESIAN_POINT('',(-20.,20.,4.));
#6074=CARTESIAN_POINT('Origin',(0.,0.,4.));
#6075=CARTESIAN_POINT('Origin',(0.,0.,0.));
#6076=CARTESIAN_POINT('',(0.,0.,0.));
#6077=CARTESIAN_POINT('Origin',(150.,0.,0.));
#6078=CARTESIAN_POINT('',(150.,0.,0.));
#6079=CARTESIAN_POINT('',(0.,150.,0.));
#6080=CARTESIAN_POINT('',(150.,0.,0.));
#6081=CARTESIAN_POINT('',(0.,150.,6.));
#6082=CARTESIAN_POINT('',(0.,150.,0.));
#6083=CARTESIAN_POINT('',(150.,0.,6.));
#6084=CARTESIAN_POINT('',(150.,0.,6.));
#6085=CARTESIAN_POINT('',(150.,0.,0.));
#6086=CARTESIAN_POINT('Origin',(0.,0.,0.));
#6087=CARTESIAN_POINT('',(0.,0.,0.));
#6088=CARTESIAN_POINT('',(0.,0.,0.));
#6089=CARTESIAN_POINT('',(0.,0.,6.));
#6090=CARTESIAN_POINT('',(0.,0.,6.));
#6091=CARTESIAN_POINT('',(0.,0.,0.));
#6092=CARTESIAN_POINT('Origin',(0.,150.,0.));
#6093=CARTESIAN_POINT('',(0.,150.,0.));
#6094=CARTESIAN_POINT('',(0.,150.,6.));
#6095=CARTESIAN_POINT('Origin',(75.,75.,6.));
#6096=CARTESIAN_POINT('Origin',(75.,75.,0.));
#6097=CARTESIAN_POINT('',(0.,0.,0.));
#6098=CARTESIAN_POINT('Origin',(0.,0.,0.));
#6099=CARTESIAN_POINT('',(-2.51487600649923,-0.00174710143214298,0.887416697508018));
#6100=CARTESIAN_POINT('',(-2.52011424653381,-0.00155468419460097,0.612583302491977));
#6101=CARTESIAN_POINT('',(-2.5175,-3.08304831685346E-16,0.));
#6102=CARTESIAN_POINT('',(1.91346599666506,-1.63598720337495,0.));
#6103=CARTESIAN_POINT('Ctrl Pts',(-2.52011424653381,-0.00155468419460097,
0.612583302491977));
#6104=CARTESIAN_POINT('Ctrl Pts',(-2.51459953682427,0.727061179433973,0.566372033576619));
#6105=CARTESIAN_POINT('Ctrl Pts',(-2.18058200222388,1.45987955194242,0.520160764661261));
#6106=CARTESIAN_POINT('Ctrl Pts',(-1.62389475685714,1.92874616523596,0.473949495745903));
#6107=CARTESIAN_POINT('Ctrl Pts',(-0.98950971657857,2.46305329699636,0.421288440663024));
#6108=CARTESIAN_POINT('Ctrl Pts',(-0.0659605128080866,2.65458641879863,
0.368627385580146));
#6109=CARTESIAN_POINT('Ctrl Pts',(0.728030814102273,2.41463261372602,0.315966330497268));
#6110=CARTESIAN_POINT('Ctrl Pts',(1.52202214101263,2.17467880865341,0.26330527541439));
#6111=CARTESIAN_POINT('Ctrl Pts',(2.18645559106287,1.50323807670592,0.210644220331512));
#6112=CARTESIAN_POINT('Ctrl Pts',(2.41964507597276,0.708853082730267,0.157983165248634));
#6113=CARTESIAN_POINT('Ctrl Pts',(2.65283456088265,-0.0855319112453835,
0.105322110165756));
#6114=CARTESIAN_POINT('Ctrl Pts',(2.45478008065218,-1.00286116724919,0.0526610550828779));
#6115=CARTESIAN_POINT('Ctrl Pts',(1.91346599666506,-1.63598720337495,-2.77555756156289E-16));
#6116=CARTESIAN_POINT('',(-1.91703660311682,-1.63861995150711,-4.84824442051532E-16));
#6117=CARTESIAN_POINT('Origin',(0.,0.,0.));
#6118=CARTESIAN_POINT('Ctrl Pts',(-1.91704123069775,-1.63862336360397,-2.77555756156289E-16));
#6119=CARTESIAN_POINT('Ctrl Pts',(-1.39386687448522,-2.24786647282135,0.0509809153588233));
#6120=CARTESIAN_POINT('Ctrl Pts',(-0.55338302340234,-2.58772319466498,0.101961830717647));
#6121=CARTESIAN_POINT('Ctrl Pts',(0.245732972111121,-2.5093256741233,0.15294274607647));
#6122=CARTESIAN_POINT('Ctrl Pts',(1.07118483308992,-2.42834446539943,0.205603801159349));
#6123=CARTESIAN_POINT('Ctrl Pts',(1.85249724960843,-1.90108656072576,0.258264856242227));
#6124=CARTESIAN_POINT('Ctrl Pts',(2.23581596847939,-1.16587048520445,0.310925911325105));
#6125=CARTESIAN_POINT('Ctrl Pts',(2.61913468735035,-0.430654409683135,0.363586966407983));
#6126=CARTESIAN_POINT('Ctrl Pts',(2.60445970857376,0.512519836685811,0.416248021490861));
#6127=CARTESIAN_POINT('Ctrl Pts',(2.19819451399913,1.23549094635129,0.468909076573739));
#6128=CARTESIAN_POINT('Ctrl Pts',(1.7919293194245,1.95846205601678,0.521570131656618));
#6129=CARTESIAN_POINT('Ctrl Pts',(0.994073909051824,2.46123002897879,0.574231186739496));
#6130=CARTESIAN_POINT('Ctrl Pts',(0.166600790821099,2.51599781963901,0.626892241822374));
#6131=CARTESIAN_POINT('Ctrl Pts',(-0.660872327409628,2.57076561029922,0.679553296905252));
#6132=CARTESIAN_POINT('Ctrl Pts',(-1.5179631534984,2.17753321865762,0.732214351988131));
#6133=CARTESIAN_POINT('Ctrl Pts',(-2.01603503865931,1.51452501467868,0.784875407071009));
#6134=CARTESIAN_POINT('Ctrl Pts',(-2.33931590060693,1.08418981599261,0.819055837216678));
#6135=CARTESIAN_POINT('Ctrl Pts',(-2.51134748918236,0.540202130103611,0.853236267362348));
#6136=CARTESIAN_POINT('Ctrl Pts',(-2.51487600649923,-0.00174710143214298,
0.887416697508018));
#6137=CARTESIAN_POINT('Origin',(0.,0.,0.));
#6138=CARTESIAN_POINT('',(-2.52149019825988,-0.000319702518148003,1.88741669750802));
#6139=CARTESIAN_POINT('',(-2.51813779298502,0.00219620146278118,1.61258330249198));
#6140=CARTESIAN_POINT('',(-2.5175,-3.08304831685346E-16,0.));
#6141=CARTESIAN_POINT('Ctrl Pts',(-2.51813779298502,0.00219620146278118,
1.61258330249198));
#6142=CARTESIAN_POINT('Ctrl Pts',(-2.51970373897608,0.174721836780657,1.60166608582343));
#6143=CARTESIAN_POINT('Ctrl Pts',(-2.50346821380307,0.346954441346066,1.59074886915489));
#6144=CARTESIAN_POINT('Ctrl Pts',(-2.46833960002055,0.515242964361496,1.57983165248634));
#6145=CARTESIAN_POINT('Ctrl Pts',(-2.29889074491847,1.32701133439546,1.52717059740347));
#6146=CARTESIAN_POINT('Ctrl Pts',(-1.68984135267922,2.04700961835622,1.47450954232059));
#6147=CARTESIAN_POINT('Ctrl Pts',(-0.917406816181398,2.34872522509939,1.42184848723771));
#6148=CARTESIAN_POINT('Ctrl Pts',(-0.144972279683573,2.65044083184256,1.36918743215483));
#6149=CARTESIAN_POINT('Ctrl Pts',(0.790847401072825,2.53387376136814,1.31652637707195));
#6150=CARTESIAN_POINT('Ctrl Pts',(1.46564413375167,2.05185297138638,1.26386532198907));
#6151=CARTESIAN_POINT('Ctrl Pts',(2.14044086643052,1.56983218140461,1.2112042669062));
#6152=CARTESIAN_POINT('Ctrl Pts',(2.5542146510318,0.7223576719155,1.15854321182332));
#6153=CARTESIAN_POINT('Ctrl Pts',(2.51930798934804,-0.106157141646233,1.10588215674044));
#6154=CARTESIAN_POINT('Ctrl Pts',(2.48440132766427,-0.934671955207963,1.05322110165756));
#6155=CARTESIAN_POINT('Ctrl Pts',(2.00081421969545,-1.74422707284231,1.00056004657468));
#6156=CARTESIAN_POINT('Ctrl Pts',(1.28786937648264,-2.16780796801704,0.947898991491806));
#6157=CARTESIAN_POINT('Ctrl Pts',(0.574924533269827,-2.59138886319177,0.895237936408928));
#6158=CARTESIAN_POINT('Ctrl Pts',(-0.367378045186977,-2.62899553590688,
0.84257688132605));
#6159=CARTESIAN_POINT('Ctrl Pts',(-1.11170282225959,-2.26331904582102,0.789915826243172));
#6160=CARTESIAN_POINT('Ctrl Pts',(-1.8560275993322,-1.89764255573516,0.737254771160294));
#6161=CARTESIAN_POINT('Ctrl Pts',(-2.40237457502062,-1.12868290284834,0.684593716077416));
#6162=CARTESIAN_POINT('Ctrl Pts',(-2.5029376244715,-0.305662505545658,0.631932660994538));
#6163=CARTESIAN_POINT('Ctrl Pts',(-2.51525431968946,-0.204861153089739,
0.625482874827017));
#6164=CARTESIAN_POINT('Ctrl Pts',(-2.52088394403914,-0.10324885163404,0.619033088659497));
#6165=CARTESIAN_POINT('Ctrl Pts',(-2.52011424653381,-0.00155468419460097,
0.612583302491977));
#6166=CARTESIAN_POINT('Ctrl Pts',(-2.51487600649923,-0.00174710143214298,
0.887416697508018));
#6167=CARTESIAN_POINT('Ctrl Pts',(-2.51678380007701,-0.29476741862348,0.905897322445226));
#6168=CARTESIAN_POINT('Ctrl Pts',(-2.46943253823011,-0.587191827768646,
0.924377947382434));
#6169=CARTESIAN_POINT('Ctrl Pts',(-2.37009511448484,-0.860734411891926,
0.942858572319643));
#6170=CARTESIAN_POINT('Ctrl Pts',(-2.08703036091644,-1.64020161816731,0.995519627402521));
#6171=CARTESIAN_POINT('Ctrl Pts',(-1.38184790954662,-2.26635201440178,1.0481806824854));
#6172=CARTESIAN_POINT('Ctrl Pts',(-0.574378778493375,-2.45524661303475,
1.10084173756828));
#6173=CARTESIAN_POINT('Ctrl Pts',(0.233090352559867,-2.64414121166772,1.15350279265116));
#6174=CARTESIAN_POINT('Ctrl Pts',(1.14284616329653,-2.39578001269919,1.20616384773403));
#6175=CARTESIAN_POINT('Ctrl Pts',(1.74230865905524,-1.82278291337913,1.25882490281691));
#6176=CARTESIAN_POINT('Ctrl Pts',(2.34177115481396,-1.24978581405907,1.31148595789979));
#6177=CARTESIAN_POINT('Ctrl Pts',(2.63094033559473,-0.352152814387476,1.36414701298267));
#6178=CARTESIAN_POINT('Ctrl Pts',(2.47866792745056,0.46301576636188,1.41680806806555));
#6179=CARTESIAN_POINT('Ctrl Pts',(2.32639551930638,1.27818434711123,1.46946912314843));
#6180=CARTESIAN_POINT('Ctrl Pts',(1.73268152223725,2.01088850893835,1.5221301782313));
#6181=CARTESIAN_POINT('Ctrl Pts',(0.966788038826866,2.32883881680251,1.57479123331418));
#6182=CARTESIAN_POINT('Ctrl Pts',(0.200894555416484,2.64678912466668,1.62745228839706));
#6183=CARTESIAN_POINT('Ctrl Pts',(-0.737178414335148,2.54998557856789,1.68011334347994));
#6184=CARTESIAN_POINT('Ctrl Pts',(-1.42200016567859,2.08232793645304,1.73277439856282));
#6185=CARTESIAN_POINT('Ctrl Pts',(-2.09234000745072,1.6245598395668,1.78432183154455));
#6186=CARTESIAN_POINT('Ctrl Pts',(-2.52002637342648,0.811456688510852,1.83586926452628));
#6187=CARTESIAN_POINT('Ctrl Pts',(-2.52149019825988,-0.000319702518148003,
1.88741669750802));
#6188=CARTESIAN_POINT('Origin',(0.,0.,0.));
#6189=CARTESIAN_POINT('',(-2.51571955069522,0.0020516094281591,2.88741669750802));
#6190=CARTESIAN_POINT('',(-2.51355581944505,-0.000494562389464492,2.61258330249198));
#6191=CARTESIAN_POINT('',(-2.5175,-3.08304831685346E-16,0.));
#6192=CARTESIAN_POINT('Ctrl Pts',(-2.51355581944505,-0.000494562389464492,
2.61258330249198));
#6193=CARTESIAN_POINT('Ctrl Pts',(-2.51275958993137,0.448550632625545,2.58429908298737));
#6194=CARTESIAN_POINT('Ctrl Pts',(-2.39795577577843,0.897975827471433,2.55601486348276));
#6195=CARTESIAN_POINT('Ctrl Pts',(-2.17158417223202,1.28155930423489,2.52773064397815));
#6196=CARTESIAN_POINT('Ctrl Pts',(-1.75011355390313,1.99573529892449,2.47506958889527));
#6197=CARTESIAN_POINT('Ctrl Pts',(-0.941893630300218,2.48167123557527,2.42240853381239));
#6198=CARTESIAN_POINT('Ctrl Pts',(-0.113465952320697,2.51898725941957,2.36974747872952));
#6199=CARTESIAN_POINT('Ctrl Pts',(0.714961725658818,2.55630328326386,2.31708642364664));
#6200=CARTESIAN_POINT('Ctrl Pts',(1.56359715801494,2.14499939430168,2.26442536856376));
#6201=CARTESIAN_POINT('Ctrl Pts',(2.04756973616912,1.47160818786419,2.21176431348088));
#6202=CARTESIAN_POINT('Ctrl Pts',(2.53154231432331,0.798216981426686,2.159103258398));
#6203=CARTESIAN_POINT('Ctrl Pts',(2.65085203827557,-0.137261542486132,2.10644220331512));
#6204=CARTESIAN_POINT('Ctrl Pts',(2.35138983004132,-0.910570496909335,2.05378114823225));
#6205=CARTESIAN_POINT('Ctrl Pts',(2.05192762180707,-1.68387945133254,2.00112009314937));
#6206=CARTESIAN_POINT('Ctrl Pts',(1.33369348138632,-2.29501883626613,1.94845903806649));
#6207=CARTESIAN_POINT('Ctrl Pts',(0.522419005839605,-2.46682921151411,1.89579798298361));
#6208=CARTESIAN_POINT('Ctrl Pts',(-0.288855469707103,-2.63863958676209,
1.84313692790073));
#6209=CARTESIAN_POINT('Ctrl Pts',(-1.19317028037977,-2.37112095232446,1.79047587281786));
#6210=CARTESIAN_POINT('Ctrl Pts',(-1.78040352673365,-1.78559240705206,1.73781481773498));
#6211=CARTESIAN_POINT('Ctrl Pts',(-2.24589685398929,-1.32145037757005,1.69607097932064));
#6212=CARTESIAN_POINT('Ctrl Pts',(-2.51215013162399,-0.65748496652123,1.65432714090631));
#6213=CARTESIAN_POINT('Ctrl Pts',(-2.51813779298502,0.00219620146278118,
1.61258330249198));
#6214=CARTESIAN_POINT('Ctrl Pts',(-2.52149019825988,-0.000319702518148003,
1.88741669750802));
#6215=CARTESIAN_POINT('Ctrl Pts',(-2.5215218224862,-0.0178571835903327,
1.88853031960916));
#6216=CARTESIAN_POINT('Ctrl Pts',(-2.52135451775278,-0.0353940454296833,
1.88964394171031));
#6217=CARTESIAN_POINT('Ctrl Pts',(-2.52098643312153,-0.0529266917933569,
1.89075756381145));
#6218=CARTESIAN_POINT('Ctrl Pts',(-2.50358041628578,-0.882011939794007,
1.94341861889433));
#6219=CARTESIAN_POINT('Ctrl Pts',(-2.03719784967901,-1.7016706976644,1.99607967397721));
#6220=CARTESIAN_POINT('Ctrl Pts',(-1.33335156767863,-2.14017435875082,2.04874072906008));
#6221=CARTESIAN_POINT('Ctrl Pts',(-0.629505285678259,-2.57867801983723,
2.10140178414296));
#6222=CARTESIAN_POINT('Ctrl Pts',(0.311804711715729,-2.63602658413966,2.15406283922584));
#6223=CARTESIAN_POINT('Ctrl Pts',(1.06367847532566,-2.28621117073127,2.20672389430872));
#6224=CARTESIAN_POINT('Ctrl Pts',(1.81555223893559,-1.93639575732288,2.2593849493916));
#6225=CARTESIAN_POINT('Ctrl Pts',(2.37798976876147,-1.17941636620366,2.31204600447447));
#6226=CARTESIAN_POINT('Ctrl Pts',(2.49591594240719,-0.358576241429396,2.36470705955735));
#6227=CARTESIAN_POINT('Ctrl Pts',(2.61384211605291,0.462263883344868,2.41736811464023));
#6228=CARTESIAN_POINT('Ctrl Pts',(2.28725693351847,1.34696474177417,2.47002916972311));
#6229=CARTESIAN_POINT('Ctrl Pts',(1.66427240295436,1.89429948580111,2.52269022480599));
#6230=CARTESIAN_POINT('Ctrl Pts',(1.04128787239026,2.44163422982805,2.57535127988887));
#6231=CARTESIAN_POINT('Ctrl Pts',(0.12190399379649,2.65160285945263,2.62801233497175));
#6232=CARTESIAN_POINT('Ctrl Pts',(-0.676922982005502,2.42898097098493,2.68067339005462));
#6233=CARTESIAN_POINT('Ctrl Pts',(-1.47574995780749,2.20635908251724,2.7333344451375));
#6234=CARTESIAN_POINT('Ctrl Pts',(-2.1540200308177,1.55114667595727,2.78599550022038));
#6235=CARTESIAN_POINT('Ctrl Pts',(-2.40412613268695,0.760493784040427,2.83865655530326));
#6236=CARTESIAN_POINT('Ctrl Pts',(-2.48131922521823,0.516465584049649,2.85490993603818));
#6237=CARTESIAN_POINT('Ctrl Pts',(-2.51772563121066,0.259535390913114,2.8711633167731));
#6238=CARTESIAN_POINT('Ctrl Pts',(-2.51571955069522,0.0020516094281591,
2.88741669750802));
#6239=CARTESIAN_POINT('Origin',(0.,0.,0.));
#6240=CARTESIAN_POINT('',(-2.51469328235907,-0.00165890949178153,3.88741669750802));
#6241=CARTESIAN_POINT('',(-2.51988725850616,-0.00173537346078306,3.61258330249198));
#6242=CARTESIAN_POINT('',(-2.5175,-3.08304831685346E-16,0.));
#6243=CARTESIAN_POINT('Ctrl Pts',(-2.51988725850616,-0.00173537346078306,
3.61258330249198));
#6244=CARTESIAN_POINT('Ctrl Pts',(-2.51420136288543,0.718396137764606,3.5669320801513));
#6245=CARTESIAN_POINT('Ctrl Pts',(-2.18921873634932,1.44301231504753,3.52128085781063));
#6246=CARTESIAN_POINT('Ctrl Pts',(-1.64418245628449,1.91176252643724,3.47562963546996));
#6247=CARTESIAN_POINT('Ctrl Pts',(-1.01545481012268,2.4524902317743,3.42296858038708));
#6248=CARTESIAN_POINT('Ctrl Pts',(-0.0939057222003969,2.65274169493656,
3.3703075253042));
#6249=CARTESIAN_POINT('Ctrl Pts',(0.702526568429994,2.42169946773059,3.31764647022132));
#6250=CARTESIAN_POINT('Ctrl Pts',(1.49895885906039,2.19065724052462,3.26498541513844));
#6251=CARTESIAN_POINT('Ctrl Pts',(2.17027435239889,1.52832132295041,3.21232436005557));
#6252=CARTESIAN_POINT('Ctrl Pts',(2.41202001637171,0.73507234206789,3.15966330497269));
#6253=CARTESIAN_POINT('Ctrl Pts',(2.65376568034452,-0.0581766388146221,
3.10700224988981));
#6254=CARTESIAN_POINT('Ctrl Pts',(2.46594151495165,-0.982338683005439,3.05434119480693));
#6255=CARTESIAN_POINT('Ctrl Pts',(1.93372898294791,-1.61829050288557,3.00168013972405));
#6256=CARTESIAN_POINT('Ctrl Pts',(1.40151645094418,-2.2542423227657,2.94901908464117));
#6257=CARTESIAN_POINT('Ctrl Pts',(0.524915552329573,-2.60198391833514,2.8963580295583));
#6258=CARTESIAN_POINT('Ctrl Pts',(-0.298520242041991,-2.50380859645435,
2.84369697447542));
#6259=CARTESIAN_POINT('Ctrl Pts',(-1.12195603641355,-2.40563327457356,2.79103591939254));
#6260=CARTESIAN_POINT('Ctrl Pts',(-1.89222672654207,-1.86154103524254,2.73837486430966));
#6261=CARTESIAN_POINT('Ctrl Pts',(-2.2600014150789,-1.11828688921283,2.68571380922678));
#6262=CARTESIAN_POINT('Ctrl Pts',(-2.43024455012818,-0.774234076709942,
2.66133697364852));
#6263=CARTESIAN_POINT('Ctrl Pts',(-2.51424205213159,-0.387505449655048,
2.63696013807025));
#6264=CARTESIAN_POINT('Ctrl Pts',(-2.51355581944505,-0.000494562389464492,
2.61258330249198));
#6265=CARTESIAN_POINT('Ctrl Pts',(-2.51571955069522,0.0020516094281591,
2.88741669750802));
#6266=CARTESIAN_POINT('Ctrl Pts',(-2.51122591781276,-0.574713669074463,
2.92382437185598));
#6267=CARTESIAN_POINT('Ctrl Pts',(-2.31399271794437,-1.15425664796212,2.96023204620393));
#6268=CARTESIAN_POINT('Ctrl Pts',(-1.95070481508442,-1.59778720918929,2.99663972055189));
#6269=CARTESIAN_POINT('Ctrl Pts',(-1.42523526488438,-2.23932193322841,3.04930077563477));
#6270=CARTESIAN_POINT('Ctrl Pts',(-0.55235403375603,-2.59629800403293,3.10196183071765));
#6271=CARTESIAN_POINT('Ctrl Pts',(0.272072347378842,-2.50682067463764,3.15462288580053));
#6272=CARTESIAN_POINT('Ctrl Pts',(1.09649872851371,-2.41734334524235,3.20728394088341));
#6273=CARTESIAN_POINT('Ctrl Pts',(1.8724702596551,-1.88141261564727,3.25994499596628));
#6274=CARTESIAN_POINT('Ctrl Pts',(2.24807060652927,-1.14208222144429,3.31260605104916));
#6275=CARTESIAN_POINT('Ctrl Pts',(2.62367095340345,-0.402751827241306,3.36526710613204));
#6276=CARTESIAN_POINT('Ctrl Pts',(2.5989001160104,0.539978231569575,3.41792816121491));
#6277=CARTESIAN_POINT('Ctrl Pts',(2.18499209295389,1.25856378644175,3.47058921629779));
#6278=CARTESIAN_POINT('Ctrl Pts',(1.77108406989738,1.97714934131393,3.52325027138067));
#6279=CARTESIAN_POINT('Ctrl Pts',(0.968038861177412,2.4715903922474,3.57591132646355));
#6280=CARTESIAN_POINT('Ctrl Pts',(0.14005117319827,2.5176494835237,3.62857238154643));
#6281=CARTESIAN_POINT('Ctrl Pts',(-0.687936514780865,2.56370857479999,3.68123343662931));
#6282=CARTESIAN_POINT('Ctrl Pts',(-1.54086668201918,2.16138570641911,3.73389449171218));
#6283=CARTESIAN_POINT('Ctrl Pts',(-2.03192094120479,1.49314116576332,3.78655554679506));
#6284=CARTESIAN_POINT('Ctrl Pts',(-2.3454245829758,1.06651397911266,3.82017593036605));
#6285=CARTESIAN_POINT('Ctrl Pts',(-2.51143030795531,0.531499105364158,3.85379631393703));
#6286=CARTESIAN_POINT('Ctrl Pts',(-2.51469328235907,-0.00165890949178153,
3.88741669750802));
#6287=CARTESIAN_POINT('Origin',(0.,0.,0.));
#6288=CARTESIAN_POINT('',(-2.52142713785251,-0.000477745744092403,4.88741669750802));
#6289=CARTESIAN_POINT('',(-2.5184009829045,0.00215602902869219,4.61258330249198));
#6290=CARTESIAN_POINT('',(-2.5175,-3.08304831685346E-16,0.));
#6291=CARTESIAN_POINT('Ctrl Pts',(-2.5184009829045,0.00215602902869219,
4.61258330249198));
#6292=CARTESIAN_POINT('Ctrl Pts',(-2.51987859619477,0.165787052272115,4.60222613239812));
#6293=CARTESIAN_POINT('Ctrl Pts',(-2.50528024663712,0.329155676438073,4.59186896230426));
#6294=CARTESIAN_POINT('Ctrl Pts',(-2.47364099272538,0.489154516809472,4.5815117922104));
#6295=CARTESIAN_POINT('Ctrl Pts',(-2.31277113368779,1.30266898742634,4.52885073712752));
#6296=CARTESIAN_POINT('Ctrl Pts',(-1.71135702808935,2.02906725622667,4.47618968204464));
#6297=CARTESIAN_POINT('Ctrl Pts',(-0.942150236578554,2.33891531144121,4.42352862696176));
#6298=CARTESIAN_POINT('Ctrl Pts',(-0.172943445067766,2.64876336665576,4.37086757187889));
#6299=CARTESIAN_POINT('Ctrl Pts',(0.764056032355369,2.54206120828453,4.31820651679601));
#6300=CARTESIAN_POINT('Ctrl Pts',(1.44390294176358,2.06720008630591,4.26554546171313));
#6301=CARTESIAN_POINT('Ctrl Pts',(2.1237498511718,1.59233896432729,4.21288440663025));
#6302=CARTESIAN_POINT('Ctrl Pts',(2.54644419256509,0.749318878741279,4.16022335154737));
#6303=CARTESIAN_POINT('Ctrl Pts',(2.52028686841065,-0.0795361749092185,
4.10756229646449));
#6304=CARTESIAN_POINT('Ctrl Pts',(2.4941295442562,-0.908391228559711,4.05490124138161));
#6305=CARTESIAN_POINT('Ctrl Pts',(2.01912055455403,-1.72308125027469,4.00224018629874));
#6306=CARTESIAN_POINT('Ctrl Pts',(1.31068458263584,-2.15413041105905,3.94957913121586));
#6307=CARTESIAN_POINT('Ctrl Pts',(0.602248610717651,-2.58517957184342,3.89691807613298));
#6308=CARTESIAN_POINT('Ctrl Pts',(-0.339614343416557,-2.63258787169717,
3.8442570210501));
#6309=CARTESIAN_POINT('Ctrl Pts',(-1.08775335610003,-2.27485483868615,3.79159596596722));
#6310=CARTESIAN_POINT('Ctrl Pts',(-1.83589236878351,-1.91712180567512,3.73893491088435));
#6311=CARTESIAN_POINT('Ctrl Pts',(-2.39030744001625,-1.15424743979932,3.68627385580147));
#6312=CARTESIAN_POINT('Ctrl Pts',(-2.49956187343194,-0.332208283105492,
3.63361280071859));
#6313=CARTESIAN_POINT('Ctrl Pts',(-2.51410497940244,-0.222784782438857,
3.62660296797639));
#6314=CARTESIAN_POINT('Ctrl Pts',(-2.52076033868337,-0.112312948107318,
3.61959313523418));
#6315=CARTESIAN_POINT('Ctrl Pts',(-2.51988725850616,-0.00173537346078306,
3.61258330249198));
#6316=CARTESIAN_POINT('Ctrl Pts',(-2.51469328235907,-0.00165890949178153,
3.88741669750802));
#6317=CARTESIAN_POINT('Ctrl Pts',(-2.51654124532602,-0.303609260634305,
3.90645736901991));
#6318=CARTESIAN_POINT('Ctrl Pts',(-2.46619036907829,-0.604964034533392,
3.92549804053181));
#6319=CARTESIAN_POINT('Ctrl Pts',(-2.36087140795563,-0.885697153183018,
3.9445387120437));
#6320=CARTESIAN_POINT('Ctrl Pts',(-2.06958926438796,-1.66212471854286,3.99719976712658));
#6321=CARTESIAN_POINT('Ctrl Pts',(-1.35784662611974,-2.28081363633185,4.04986082220945));
#6322=CARTESIAN_POINT('Ctrl Pts',(-0.548430926173578,-2.46117792359562,
4.10252187729233));
#6323=CARTESIAN_POINT('Ctrl Pts',(0.260984773772587,-2.64154221085939,4.15518293237521));
#6324=CARTESIAN_POINT('Ctrl Pts',(1.16807353539669,-2.38358186759794,4.20784398745809));
#6325=CARTESIAN_POINT('Ctrl Pts',(1.76145512481594,-1.8042863119436,4.26050504254097));
#6326=CARTESIAN_POINT('Ctrl Pts',(2.35483671423518,-1.22499075628926,4.31316609762385));
#6327=CARTESIAN_POINT('Ctrl Pts',(2.63451113144957,-0.32435998824203,4.36582715270673));
#6328=CARTESIAN_POINT('Ctrl Pts',(2.47364125533363,0.489154568739605,4.41848820778961));
#6329=CARTESIAN_POINT('Ctrl Pts',(2.31277137921768,1.30266912572123,4.47114926287248));
#6330=CARTESIAN_POINT('Ctrl Pts',(1.71135720977141,2.02906747163727,4.52381031795536));
#6331=CARTESIAN_POINT('Ctrl Pts',(0.942150336599642,2.33891555974628,4.57647137303824));
#6332=CARTESIAN_POINT('Ctrl Pts',(0.172943463427865,2.64876364785529,4.62913242812111));
#6333=CARTESIAN_POINT('Ctrl Pts',(-0.764056113469408,2.54206147815727,4.68179348320399));
#6334=CARTESIAN_POINT('Ctrl Pts',(-1.44390309505201,2.06720030576578,4.73445453828687));
#6335=CARTESIAN_POINT('Ctrl Pts',(-2.10214324411594,1.60743112627774,4.78544192469392));
#6336=CARTESIAN_POINT('Ctrl Pts',(-2.51931664968783,0.802532659807444,4.83642931110097));
#6337=CARTESIAN_POINT('Ctrl Pts',(-2.52142713785251,-0.000477745744092403,
4.88741669750802));
#6338=CARTESIAN_POINT('Origin',(0.,0.,0.));
#6339=CARTESIAN_POINT('',(-2.51595242716893,0.00210630723253068,5.88741669750802));
#6340=CARTESIAN_POINT('',(-2.51351075839737,-0.000354205898239757,5.61258330249198));
#6341=CARTESIAN_POINT('',(-2.5175,-3.08304831685346E-16,0.));
#6342=CARTESIAN_POINT('Ctrl Pts',(-2.51351075839737,-0.000354205898239757,
5.61258330249198));
#6343=CARTESIAN_POINT('Ctrl Pts',(-2.51295240495751,0.439819286417837,5.58485912956205));
#6344=CARTESIAN_POINT('Ctrl Pts',(-2.40289969386439,0.880253950489353,5.55713495663213));
#6345=CARTESIAN_POINT('Ctrl Pts',(-2.18499186098815,1.25856365282659,5.5294107837022));
#6346=CARTESIAN_POINT('Ctrl Pts',(-1.77108388187219,1.97714913140962,5.47674972861932));
#6347=CARTESIAN_POINT('Ctrl Pts',(-0.968038758408038,2.47159012985723,5.42408867353645));
#6348=CARTESIAN_POINT('Ctrl Pts',(-0.14005115833078,2.51764921624498,5.37142761845357));
#6349=CARTESIAN_POINT('Ctrl Pts',(0.687936441746484,2.56370830263272,5.3187665633707));
#6350=CARTESIAN_POINT('Ctrl Pts',(1.54086651843685,2.16138547696059,5.26610550828782));
#6351=CARTESIAN_POINT('Ctrl Pts',(2.03192072549116,1.49314100724674,5.21344445320494));
#6352=CARTESIAN_POINT('Ctrl Pts',(2.52297493254547,0.82489653753288,5.16078339812206));
#6353=CARTESIAN_POINT('Ctrl Pts',(2.65215326996372,-0.109269576222705,5.10812234303918));
#6354=CARTESIAN_POINT('Ctrl Pts',(2.36087115731916,-0.885697059154641,5.0554612879563));
#6355=CARTESIAN_POINT('Ctrl Pts',(2.0695890446746,-1.66212454208657,5.00280023287342));
#6356=CARTESIAN_POINT('Ctrl Pts',(1.35784648196724,-2.28081339419485,4.95013917779055));
#6357=CARTESIAN_POINT('Ctrl Pts',(0.548430867950845,-2.46117766231084,4.89747812270767));
#6358=CARTESIAN_POINT('Ctrl Pts',(-0.260984746065556,-2.64154193042683,
4.84481706762479));
#6359=CARTESIAN_POINT('Ctrl Pts',(-1.16807341139099,-2.38358161455052,4.79215601254191));
#6360=CARTESIAN_POINT('Ctrl Pts',(-1.76145493781535,-1.80428612039566,4.73949495745903));
#6361=CARTESIAN_POINT('Ctrl Pts',(-2.23813250929503,-1.33892419551938,4.69719107247001));
#6362=CARTESIAN_POINT('Ctrl Pts',(-2.5123656680334,-0.666195260483231,4.65488718748099));
#6363=CARTESIAN_POINT('Ctrl Pts',(-2.5184009829045,0.00215602902869219,
4.61258330249198));
#6364=CARTESIAN_POINT('Ctrl Pts',(-2.52142713785251,-0.000477745744092403,
4.88741669750802));
#6365=CARTESIAN_POINT('Ctrl Pts',(-2.52149641494594,-0.0268366838431701,
4.88909036618385));
#6366=CARTESIAN_POINT('Ctrl Pts',(-2.52111846566354,-0.0531935875744284,
4.89076403485968));
#6367=CARTESIAN_POINT('Ctrl Pts',(-2.52028713597104,-0.0795361833539025,
4.89243770353551));
#6368=CARTESIAN_POINT('Ctrl Pts',(-2.49412980903954,-0.9083913249971,4.94509875861839));
#6369=CARTESIAN_POINT('Ctrl Pts',(-2.01912076890865,-1.72308143319855,4.99775981370126));
#6370=CARTESIAN_POINT('Ctrl Pts',(-1.31068472178129,-2.15413063974552,5.05042086878414));
#6371=CARTESIAN_POINT('Ctrl Pts',(-0.602248674653905,-2.58517984629251,
5.10308192386702));
#6372=CARTESIAN_POINT('Ctrl Pts',(0.339614379469953,-2.632588151185,5.15574297894989));
#6373=CARTESIAN_POINT('Ctrl Pts',(1.08775347157826,-2.27485508019369,5.20840403403277));
#6374=CARTESIAN_POINT('Ctrl Pts',(1.83589256368657,-1.91712200920239,5.26106508911565));
#6375=CARTESIAN_POINT('Ctrl Pts',(2.39030769377933,-1.1542475623273,5.31372614419854));
#6376=CARTESIAN_POINT('Ctrl Pts',(2.49956213879293,-0.332208318368038,5.36638719928141));
#6377=CARTESIAN_POINT('Ctrl Pts',(2.60881658380653,0.489830925591221,5.4190482543643));
#6378=CARTESIAN_POINT('Ctrl Pts',(2.27291034374099,1.37103496663465,5.47170930944717));
#6379=CARTESIAN_POINT('Ctrl Pts',(1.64418263083336,1.91176272938481,5.52437036453004));
#6380=CARTESIAN_POINT('Ctrl Pts',(1.01545491792572,2.45249049213496,5.57703141961292));
#6381=CARTESIAN_POINT('Ctrl Pts',(0.0939057321760005,2.65274197659184,5.6296924746958));
#6382=CARTESIAN_POINT('Ctrl Pts',(-0.70252664300866,2.42169972484316,5.68235352977868));
#6383=CARTESIAN_POINT('Ctrl Pts',(-1.49895901819332,2.19065747309447,5.73501458486156));
#6384=CARTESIAN_POINT('Ctrl Pts',(-2.17027458281292,1.52832148514024,5.78767563994444));
#6385=CARTESIAN_POINT('Ctrl Pts',(-2.41202027244453,0.735072420070988,5.84033669502731));
#6386=CARTESIAN_POINT('Ctrl Pts',(-2.48406204758965,0.498679080992718,5.85603002918755));
#6387=CARTESIAN_POINT('Ctrl Pts',(-2.51795464778859,0.250659633631731,5.87172336334778));
#6388=CARTESIAN_POINT('Ctrl Pts',(-2.51595242716893,0.00210630723253068,
5.88741669750802));
#6389=CARTESIAN_POINT('Origin',(0.,0.,0.));
#6390=CARTESIAN_POINT('',(-2.51451849661665,-0.00155877597875643,6.88741669750802));
#6391=CARTESIAN_POINT('',(-2.51965512385738,-0.00182887343565974,6.61258330249198));
#6392=CARTESIAN_POINT('',(-2.5175,-3.08304831685346E-16,0.));
#6393=CARTESIAN_POINT('Ctrl Pts',(-2.51965512385738,-0.00182887343565974,
6.61258330249198));
#6394=CARTESIAN_POINT('Ctrl Pts',(-2.51382586072417,0.70963927099582,6.56749212672599));
#6395=CARTESIAN_POINT('Ctrl Pts',(-2.19770441709654,1.42564242834162,6.52240095096));
#6396=CARTESIAN_POINT('Ctrl Pts',(-1.66427222622564,1.89429928459087,6.47730977519401));
#6397=CARTESIAN_POINT('Ctrl Pts',(-1.04128776176594,2.44163397042813,6.42464872011113));
#6398=CARTESIAN_POINT('Ctrl Pts',(-0.121903980861276,2.65160257796401,6.37198766502826));
#6399=CARTESIAN_POINT('Ctrl Pts',(0.676922910116403,2.4289807131762,6.31932660994538));
#6400=CARTESIAN_POINT('Ctrl Pts',(1.47574980109409,2.20635884838837,6.2666655548625));
#6401=CARTESIAN_POINT('Ctrl Pts',(2.15401980214479,1.55114651127684,6.21400449977962));
#6402=CARTESIAN_POINT('Ctrl Pts',(2.40412587747264,0.760493703272659,6.16134344469674));
#6403=CARTESIAN_POINT('Ctrl Pts',(2.65423195280049,-0.0301591047315269,
6.10868238961386));
#6404=CARTESIAN_POINT('Ctrl Pts',(2.47617410240549,-0.956252383628369,6.05602133453099));
#6405=CARTESIAN_POINT('Ctrl Pts',(1.95070460798478,-1.59778703954676,6.00336027944811));
#6406=CARTESIAN_POINT('Ctrl Pts',(1.42523511356408,-2.23932169546514,5.95069922436523));
#6407=CARTESIAN_POINT('Ctrl Pts',(0.552353975117676,-2.59629772840507,5.89803816928235));
#6408=CARTESIAN_POINT('Ctrl Pts',(-0.272072318490672,-2.50682040851643,
5.84537711419947));
#6409=CARTESIAN_POINT('Ctrl Pts',(-1.09649861209903,-2.4173430886278,5.79271605911659));
#6410=CARTESIAN_POINT('Ctrl Pts',(-1.87247006086932,-1.88141241591059,5.74005500403372));
#6411=CARTESIAN_POINT('Ctrl Pts',(-2.24807036787059,-1.14208210019275,5.68739394895084));
#6412=CARTESIAN_POINT('Ctrl Pts',(-2.42593046918386,-0.791982905899236,
5.66245706679789));
#6413=CARTESIAN_POINT('Ctrl Pts',(-2.5140129769474,-0.396274204395027,5.63752018464493));
#6414=CARTESIAN_POINT('Ctrl Pts',(-2.51351075839737,-0.000354205898239757,
5.61258330249198));
#6415=CARTESIAN_POINT('Ctrl Pts',(-2.51595242716893,0.00210630723253068,
5.88741669750802));
#6416=CARTESIAN_POINT('Ctrl Pts',(-2.51123593210567,-0.583393874621885,
5.92438441843066));
#6417=CARTESIAN_POINT('Ctrl Pts',(-2.30733899175125,-1.17185655251717,5.9613521393533));
#6418=CARTESIAN_POINT('Ctrl Pts',(-1.93372918822543,-1.61829067462528,5.99831986027594));
#6419=CARTESIAN_POINT('Ctrl Pts',(-1.40151659973107,-2.25424256206805,6.05098091535882));
#6420=CARTESIAN_POINT('Ctrl Pts',(-0.524915608098723,-2.60198419476933,
6.1036419704417));
#6421=CARTESIAN_POINT('Ctrl Pts',(0.298520273710652,-2.50380886237859,6.15630302552458));
#6422=CARTESIAN_POINT('Ctrl Pts',(1.12195615552003,-2.40563352998785,6.20896408060746));
#6423=CARTESIAN_POINT('Ctrl Pts',(1.89222692750642,-1.8615412325051,6.26162513569033));
#6424=CARTESIAN_POINT('Ctrl Pts',(2.26000165505001,-1.11828700772708,6.31428619077321));
#6425=CARTESIAN_POINT('Ctrl Pts',(2.62777638259361,-0.375032782949049,6.36694724585609));
#6426=CARTESIAN_POINT('Ctrl Pts',(2.59305506569438,0.567383369124259,6.41960830093898));
#6427=CARTESIAN_POINT('Ctrl Pts',(2.17158440269112,1.28155943991538,6.47226935602186));
#6428=CARTESIAN_POINT('Ctrl Pts',(1.75011373968786,1.99573551070649,6.52493041110473));
#6429=CARTESIAN_POINT('Ctrl Pts',(0.941893730580582,2.48167150021543,6.57759146618761));
#6430=CARTESIAN_POINT('Ctrl Pts',(0.11346596452102,2.51898752751594,6.63025252127048));
#6431=CARTESIAN_POINT('Ctrl Pts',(-0.714961801538553,2.55630355481645,6.68291357635336));
#6432=CARTESIAN_POINT('Ctrl Pts',(-1.56359732455041,2.14499961990851,6.73557463143624));
#6433=CARTESIAN_POINT('Ctrl Pts',(-2.04756995383571,1.47160834288076,6.78823568651912));
#6434=CARTESIAN_POINT('Ctrl Pts',(-2.35140545800432,1.04885679500788,6.82129602351542));
#6435=CARTESIAN_POINT('Ctrl Pts',(-2.51151771720726,0.522809727020648,6.85435636051172));
#6436=CARTESIAN_POINT('Ctrl Pts',(-2.51451849661665,-0.00155877597875643,
6.88741669750802));
#6437=CARTESIAN_POINT('Origin',(0.,0.,0.));
#6438=CARTESIAN_POINT('',(-2.52134266056864,-0.000655147898209446,7.88741669750802));
#6439=CARTESIAN_POINT('',(-2.5186623288877,0.00210982157644382,7.61258330249198));
#6440=CARTESIAN_POINT('',(-2.5175,-3.08304831685346E-16,0.));
#6441=CARTESIAN_POINT('Ctrl Pts',(-2.5186623288877,0.00210982157644382,
7.61258330249198));
#6442=CARTESIAN_POINT('Ctrl Pts',(-2.52004665861774,0.156851743540232,7.6027861789728));
#6443=CARTESIAN_POINT('Ctrl Pts',(-2.50699659804811,0.311360834758803,7.59298905545363));
#6444=CARTESIAN_POINT('Ctrl Pts',(-2.4786676666043,0.463015723985691,7.58319193193445));
#6445=CARTESIAN_POINT('Ctrl Pts',(-2.32639527601114,1.27818422314105,7.53053087685157));
#6446=CARTESIAN_POINT('Ctrl Pts',(-1.73268133779952,2.01088829447311,7.47786982176869));
#6447=CARTESIAN_POINT('Ctrl Pts',(-0.966787934844472,2.32883856578358,7.42520876668581));
#6448=CARTESIAN_POINT('Ctrl Pts',(-0.200894531889431,2.64678883709404,7.37254771160294));
#6449=CARTESIAN_POINT('Ctrl Pts',(0.737178335809047,2.54998530838289,7.31988665652006));
#6450=CARTESIAN_POINT('Ctrl Pts',(1.4220000139359,2.08232771749063,7.26722560143718));
#6451=CARTESIAN_POINT('Ctrl Pts',(2.10682169206276,1.61467012659837,7.2145645463543));
#6452=CARTESIAN_POINT('Ctrl Pts',(2.53839218061801,0.776158473525024,7.16190349127142));
#6453=CARTESIAN_POINT('Ctrl Pts',(2.52098616593426,-0.0529266873392757,
7.10924243618854));
#6454=CARTESIAN_POINT('Ctrl Pts',(2.5035801512505,-0.882011848203581,7.05658138110567));
#6455=CARTESIAN_POINT('Ctrl Pts',(2.03719763332772,-1.70167051685883,7.00392032602279));
#6456=CARTESIAN_POINT('Ctrl Pts',(1.33335142587202,-2.14017413090131,6.95125927093991));
#6457=CARTESIAN_POINT('Ctrl Pts',(0.629505218416328,-2.57867774494379,6.89859821585704));
#6458=CARTESIAN_POINT('Ctrl Pts',(-0.31180467857228,-2.63602630437352,6.84593716077416));
#6459=CARTESIAN_POINT('Ctrl Pts',(-1.0636783622589,-2.28621092837513,6.79327610569128));
#6460=CARTESIAN_POINT('Ctrl Pts',(-1.81555204594553,-1.93639555237673,6.7406150506084));
#6461=CARTESIAN_POINT('Ctrl Pts',(-2.37798951633018,-1.17941624095021,6.68795399552552));
#6462=CARTESIAN_POINT('Ctrl Pts',(-2.49591567751513,-0.358576203167625,
6.63529294044265));
#6463=CARTESIAN_POINT('Ctrl Pts',(-2.51286723321544,-0.240582744534753,
6.62772306112576));
#6464=CARTESIAN_POINT('Ctrl Pts',(-2.5206337370267,-0.121269715233796,6.62015318180887));
#6465=CARTESIAN_POINT('Ctrl Pts',(-2.51965512385738,-0.00182887343565974,
6.61258330249198));
#6466=CARTESIAN_POINT('Ctrl Pts',(-2.51451849661665,-0.00155877597875643,
6.88741669750802));
#6467=CARTESIAN_POINT('Ctrl Pts',(-2.51629759013436,-0.312444874989867,
6.9070174155946));
#6468=CARTESIAN_POINT('Ctrl Pts',(-2.4628514793145,-0.622740952860776,6.92661813368118));
#6469=CARTESIAN_POINT('Ctrl Pts',(-2.35139007912217,-0.910570591403298,
6.94621885176775));
#6470=CARTESIAN_POINT('Ctrl Pts',(-2.0519278395646,-1.68387962951205,6.99887990685063));
#6471=CARTESIAN_POINT('Ctrl Pts',(-1.33369362489071,-2.295019086582,7.05154096193351));
#6472=CARTESIAN_POINT('Ctrl Pts',(-0.522419062335059,-2.46682947727924,
7.10420201701639));
#6473=CARTESIAN_POINT('Ctrl Pts',(0.288855500220588,-2.63863986797649,7.15686307209927));
#6474=CARTESIAN_POINT('Ctrl Pts',(1.193170410658,-2.37112119230105,7.20952412718215));
#6475=CARTESIAN_POINT('Ctrl Pts',(1.78040371769394,-1.78559258972849,7.26218518226502));
#6476=CARTESIAN_POINT('Ctrl Pts',(2.36763702472988,-1.20006398715593,7.3148462373479));
#6477=CARTESIAN_POINT('Ctrl Pts',(2.63778872836434,-0.296525457686245,7.36750729243078));
#6478=CARTESIAN_POINT('Ctrl Pts',(2.4683398583974,0.515243006912746,7.42016834751366));
#6479=CARTESIAN_POINT('Ctrl Pts',(2.29889098843046,1.32701147151174,7.47282940259653));
#6480=CARTESIAN_POINT('Ctrl Pts',(1.68984154486212,2.04700987124004,7.52549045767942));
#6481=CARTESIAN_POINT('Ctrl Pts',(0.917406920482627,2.34872549572162,7.57815151276229));
#6482=CARTESIAN_POINT('Ctrl Pts',(0.144972296103131,2.6504411202032,7.63081256784517));
#6483=CARTESIAN_POINT('Ctrl Pts',(-0.790847509087517,2.53387396943805,7.68347362292805));
#6484=CARTESIAN_POINT('Ctrl Pts',(-1.46564430234878,2.05185315227782,7.73613467801093));
#6485=CARTESIAN_POINT('Ctrl Pts',(-2.11181835180565,1.59027813227568,7.78656201784329));
#6486=CARTESIAN_POINT('Ctrl Pts',(-2.51864329962567,0.793594701352211,7.83698935767566));
#6487=CARTESIAN_POINT('Ctrl Pts',(-2.52134266056864,-0.000655147898209446,
7.88741669750802));
#6488=CARTESIAN_POINT('Origin',(0.,0.,0.));
#6489=CARTESIAN_POINT('',(-2.51592828109546,0.00320694493696498,8.88741669750802));
#6490=CARTESIAN_POINT('',(-2.51342302570288,-0.000307789261743824,8.61258330249198));
#6491=CARTESIAN_POINT('',(-2.5175,-3.08304831685346E-16,0.));
#6492=CARTESIAN_POINT('',(-1.91346599666506,-1.63598720337495,9.));
#6493=CARTESIAN_POINT('Ctrl Pts',(-2.51592828109546,0.00320694493696498,
8.88741669750802));
#6494=CARTESIAN_POINT('Ctrl Pts',(-2.51065601785214,-0.589289396470771,
8.92494446500535));
#6495=CARTESIAN_POINT('Ctrl Pts',(-2.29922182808405,-1.18480356030443,8.96247223250267));
#6496=CARTESIAN_POINT('Ctrl Pts',(-1.91346599666504,-1.63598720337498,9.));
#6497=CARTESIAN_POINT('',(1.91703628304852,-1.63862073901331,9.));
#6498=CARTESIAN_POINT('Origin',(0.,0.,9.));
#6499=CARTESIAN_POINT('Ctrl Pts',(1.91704088636911,-1.63862413454171,9.));
#6500=CARTESIAN_POINT('Ctrl Pts',(1.39386644228135,-2.2478675793879,8.94901908464117));
#6501=CARTESIAN_POINT('Ctrl Pts',(0.553382875999586,-2.58772269472312,8.89803816928235));
#6502=CARTESIAN_POINT('Ctrl Pts',(-0.245732947937194,-2.50932486329663,
8.84705725392353));
#6503=CARTESIAN_POINT('Ctrl Pts',(-1.0711846316848,-2.42834333344235,8.79439619884064));
#6504=CARTESIAN_POINT('Ctrl Pts',(-1.85249699178243,-1.90108649006683,8.74173514375777));
#6505=CARTESIAN_POINT('Ctrl Pts',(-2.23581570064333,-1.16587069267918,8.68907408867489));
#6506=CARTESIAN_POINT('Ctrl Pts',(-2.42140730689609,-0.80990090141839,8.66357715994725));
#6507=CARTESIAN_POINT('Ctrl Pts',(-2.51370081905187,-0.40518115145991,8.63808023121962));
#6508=CARTESIAN_POINT('Ctrl Pts',(-2.51342302570288,-0.000307789261743824,
8.61258330249198));
#6509=CARTESIAN_POINT('Origin',(0.,0.,-2.20842344717745));
#6510=CARTESIAN_POINT('',(-3.07819132760982,-0.00079983994656474,8.20842344717746));
#6511=CARTESIAN_POINT('',(-3.0685226095324,-0.00037576575812523,8.29157655282255));
#6512=CARTESIAN_POINT('',(-3.0735,-1.43456032168185E-13,-2.20842344717745));
#6513=CARTESIAN_POINT('',(0.793799282532882,2.96922295374569,9.));
#6514=CARTESIAN_POINT('Ctrl Pts',(-3.0685226095324,-0.000375765758125098,
8.29157655282255));
#6515=CARTESIAN_POINT('Ctrl Pts',(-3.06886175465975,-0.494667038336489,
8.31707348155019));
#6516=CARTESIAN_POINT('Ctrl Pts',(-2.72346330097092,-2.00928678297278,8.39523146536071));
#6517=CARTESIAN_POINT('Ctrl Pts',(-0.353891728589143,-3.60835636284,8.52605050425409));
#6518=CARTESIAN_POINT('Ctrl Pts',(2.83103930764092,-2.27044520800339,8.68403366950274));
#6519=CARTESIAN_POINT('Ctrl Pts',(3.44352590057726,1.13463251498715,8.84201683475136));
#6520=CARTESIAN_POINT('Ctrl Pts',(1.77625330176034,2.70657130793361,8.94733894491712));
#6521=CARTESIAN_POINT('Ctrl Pts',(0.793799282532882,2.96922295374569,9.));
#6522=CARTESIAN_POINT('',(-0.793799282532857,2.9692229537457,9.));
#6523=CARTESIAN_POINT('Origin',(0.,0.,9.));
#6524=CARTESIAN_POINT('Ctrl Pts',(-3.07819132760982,-0.000799839946564419,
8.20842344717746));
#6525=CARTESIAN_POINT('Ctrl Pts',(-3.07833730528696,-0.0437517646857214,
8.21065716242797));
#6526=CARTESIAN_POINT('Ctrl Pts',(-3.05813411202838,-1.09917547321831,8.26555193276136));
#6527=CARTESIAN_POINT('Ctrl Pts',(-1.85231323033622,-3.11779603581512,8.37310775817763));
#6528=CARTESIAN_POINT('Ctrl Pts',(1.59892942568934,-3.25553164520284,8.53109092342626));
#6529=CARTESIAN_POINT('Ctrl Pts',(3.59995819558759,-0.439170790472673,8.68907408867489));
#6530=CARTESIAN_POINT('Ctrl Pts',(2.34901404634718,2.73903334879023,8.84537711419948));
#6531=CARTESIAN_POINT('Ctrl Pts',(0.15211409622113,3.22551487048637,8.94901908464117));
#6532=CARTESIAN_POINT('Ctrl Pts',(-0.795573338178512,2.9743476420004,8.99999999999999));
#6533=CARTESIAN_POINT('Origin',(0.,0.,-2.20842344717745));
#6534=CARTESIAN_POINT('',(-3.06986001960329,-0.00190303792297591,7.20842344717746));
#6535=CARTESIAN_POINT('',(-3.07491903389726,0.00257578415689406,7.29157655282255));
#6536=CARTESIAN_POINT('',(-3.0735,-1.43456032168185E-13,-2.20842344717745));
#6537=CARTESIAN_POINT('Ctrl Pts',(-3.07491903389726,0.00257578415689394,
7.29157655282255));
#6538=CARTESIAN_POINT('Ctrl Pts',(-3.06752474008062,-0.823966629777171,
7.33444048438625));
#6539=CARTESIAN_POINT('Ctrl Pts',(-2.2992951061863,-2.67809470862681,7.42996547103282));
#6540=CARTESIAN_POINT('Ctrl Pts',(0.826109632836259,-3.5313227329181,7.57815151276229));
#6541=CARTESIAN_POINT('Ctrl Pts',(3.40888391949913,-1.23800854484421,7.73613467801092));
#6542=CARTESIAN_POINT('Ctrl Pts',(2.89959383691459,2.17837089371843,7.89411784325955));
#6543=CARTESIAN_POINT('Ctrl Pts',(-0.239554039779309,3.61860800891848,8.0521010085082));
#6544=CARTESIAN_POINT('Ctrl Pts',(-2.69013535674363,2.07437726859049,8.18458724502919));
#6545=CARTESIAN_POINT('Ctrl Pts',(-3.06816128832425,0.526236310858699,8.26441242646731));
#6546=CARTESIAN_POINT('Ctrl Pts',(-3.0685226095324,-0.000375765758125098,
8.29157655282255));
#6547=CARTESIAN_POINT('Ctrl Pts',(-3.06986001960329,-0.00190303792297591,
7.20842344717746));
#6548=CARTESIAN_POINT('Ctrl Pts',(-3.07203203307961,-0.381449582236985,
7.22802416526404));
#6549=CARTESIAN_POINT('Ctrl Pts',(-2.83147587564289,-1.7780644343801,7.30028593843349));
#6550=CARTESIAN_POINT('Ctrl Pts',(-0.751386096246847,-3.5479953461427,7.42520876668581));
#6551=CARTESIAN_POINT('Ctrl Pts',(2.56072339002455,-2.56819159278999,7.58319193193446));
#6552=CARTESIAN_POINT('Ctrl Pts',(3.55017077169744,0.741074350000556,7.74117509718308));
#6553=CARTESIAN_POINT('Ctrl Pts',(1.31948938364505,3.37811317609581,7.89915826243173));
#6554=CARTESIAN_POINT('Ctrl Pts',(-2.05954752837555,2.95721515386999,8.05490771242984));
#6555=CARTESIAN_POINT('Ctrl Pts',(-3.07489580194622,0.968863282862285,8.1579961073451));
#6556=CARTESIAN_POINT('Ctrl Pts',(-3.07819132760982,-0.000799839946564419,
8.20842344717746));
#6557=CARTESIAN_POINT('Origin',(0.,0.,-2.20842344717745));
#6558=CARTESIAN_POINT('',(-3.07161063948509,0.00257149365592749,6.20842344717746));
#6559=CARTESIAN_POINT('',(-3.07613109162886,-0.00223278748941785,6.29157655282255));
#6560=CARTESIAN_POINT('',(-3.0735,-1.43456032168185E-13,-2.20842344717745));
#6561=CARTESIAN_POINT('Ctrl Pts',(-3.07613109162887,-0.00223278748941807,
6.29157655282255));
#6562=CARTESIAN_POINT('Ctrl Pts',(-3.07732583545246,-0.148052619571458,
6.29914643213944));
#6563=CARTESIAN_POINT('Ctrl Pts',(-3.00188266295528,-1.30704946930654,6.3593773665392));
#6564=CARTESIAN_POINT('Ctrl Pts',(-1.5298699694087,-3.288217534816,6.47226935602186));
#6565=CARTESIAN_POINT('Ctrl Pts',(1.91773595122029,-3.07817487653525,6.63025252127048));
#6566=CARTESIAN_POINT('Ctrl Pts',(3.62589086939586,-0.0761241300265441,
6.78823568651912));
#6567=CARTESIAN_POINT('Ctrl Pts',(2.04523716940625,2.99497684203422,6.94621885176775));
#6568=CARTESIAN_POINT('Ctrl Pts',(-1.39051293053958,3.34952577410217,7.10420201701639));
#6569=CARTESIAN_POINT('Ctrl Pts',(-2.97503873711316,1.39405793869258,7.21932125070132));
#6570=CARTESIAN_POINT('Ctrl Pts',(-3.07660909841575,0.191493081934767,7.28177942930337));
#6571=CARTESIAN_POINT('Ctrl Pts',(-3.07491903389726,0.00257578415689394,
7.29157655282255));
#6572=CARTESIAN_POINT('Ctrl Pts',(-3.07161063948509,0.00257149365592728,
6.20842344717746));
#6573=CARTESIAN_POINT('Ctrl Pts',(-3.06585248751805,-0.712238758153184,
6.2453911681001));
#6574=CARTESIAN_POINT('Ctrl Pts',(-2.46232196902915,-2.45407551393839,6.33501994410562));
#6575=CARTESIAN_POINT('Ctrl Pts',(0.429356514911867,-3.60118463981366,6.47730977519402));
#6576=CARTESIAN_POINT('Ctrl Pts',(3.25052102458439,-1.60841283090018,6.63529294044265));
#6577=CARTESIAN_POINT('Ctrl Pts',(3.12335204644367,1.8432448176368,6.79327610569127));
#6578=CARTESIAN_POINT('Ctrl Pts',(0.163196100475927,3.6230155390935,6.95125927093992));
#6579=CARTESIAN_POINT('Ctrl Pts',(-2.55935722897219,2.3034892324118,7.08964171810198));
#6580=CARTESIAN_POINT('Ctrl Pts',(-3.06619650599269,0.638274357893825,7.17536311018116));
#6581=CARTESIAN_POINT('Ctrl Pts',(-3.06986001960329,-0.00190303792297591,
7.20842344717746));
#6582=CARTESIAN_POINT('Origin',(0.,0.,-2.20842344717745));
#6583=CARTESIAN_POINT('',(-3.07829446204158,-0.000583257813248639,5.20842344717746));
#6584=CARTESIAN_POINT('',(-3.06862971834531,-0.000432433695449898,5.29157655282255));
#6585=CARTESIAN_POINT('',(-3.0735,-1.43456032168185E-13,-2.20842344717745));
#6586=CARTESIAN_POINT('Ctrl Pts',(-3.06862971834531,-0.000432433695450388,
5.29157655282255));
#6587=CARTESIAN_POINT('Ctrl Pts',(-3.06924285388195,-0.483792956189932,
5.3165134349755));
#6588=CARTESIAN_POINT('Ctrl Pts',(-2.73461550492184,-1.98709885774611,5.39411137221133));
#6589=CARTESIAN_POINT('Ctrl Pts',(-0.391316876461119,-3.60551614915347,
5.52437036453005));
#6590=CARTESIAN_POINT('Ctrl Pts',(2.80566446893912,-2.29806927260028,5.68235352977867));
#6591=CARTESIAN_POINT('Ctrl Pts',(3.45781239726766,1.09380483983996,5.84033669502732));
#6592=CARTESIAN_POINT('Ctrl Pts',(0.97360642122477,3.49356069061924,5.99831986027594));
#6593=CARTESIAN_POINT('Ctrl Pts',(-2.23234707976449,2.76138593791136,6.1487331462077));
#6594=CARTESIAN_POINT('Ctrl Pts',(-3.06901441228829,0.866365958055841,6.24648537705656));
#6595=CARTESIAN_POINT('Ctrl Pts',(-3.07613109162887,-0.00223278748941807,
6.29157655282255));
#6596=CARTESIAN_POINT('Ctrl Pts',(-3.07829446204158,-0.000583257813248778,
5.20842344717746));
#6597=CARTESIAN_POINT('Ctrl Pts',(-3.07837903925972,-0.0327636734030677,
5.21009711585329));
#6598=CARTESIAN_POINT('Ctrl Pts',(-3.06339926603453,-1.07740235694415,5.26443183961199));
#6599=CARTESIAN_POINT('Ctrl Pts',(-1.88513501425953,-3.09824859284726,5.37142761845357));
#6600=CARTESIAN_POINT('Ctrl Pts',(1.56449687870927,-3.27188445193808,5.52941078370221));
#6601=CARTESIAN_POINT('Ctrl Pts',(3.59507670274909,-0.477809442042676,5.68739394895084));
#6602=CARTESIAN_POINT('Ctrl Pts',(2.36479925030647,2.74965505068462,5.84537711419948));
#6603=CARTESIAN_POINT('Ctrl Pts',(-1.01043183895086,3.48308854122473,6.00336027944811));
#6604=CARTESIAN_POINT('Ctrl Pts',(-2.89382807597609,1.62488477968039,6.1243757237741));
#6605=CARTESIAN_POINT('Ctrl Pts',(-3.07405505858123,0.306018821833909,6.19273011301722));
#6606=CARTESIAN_POINT('Ctrl Pts',(-3.07161063948509,0.00257149365592728,
6.20842344717746));
#6607=CARTESIAN_POINT('Origin',(0.,0.,-2.20842344717745));
#6608=CARTESIAN_POINT('',(-3.07007340747988,-0.00202528632500865,4.20842344717746));
#6609=CARTESIAN_POINT('',(-3.07459996860257,0.00263219671087622,4.29157655282255));
#6610=CARTESIAN_POINT('',(-3.0735,-1.43456032168185E-13,-2.20842344717745));
#6611=CARTESIAN_POINT('Ctrl Pts',(-3.07459996860257,0.00263219671087611,
4.29157655282254));
#6612=CARTESIAN_POINT('Ctrl Pts',(-3.06723173016907,-0.813327163096425,
4.33388043781156));
#6613=CARTESIAN_POINT('Ctrl Pts',(-2.31566637879303,-2.65701288209306,4.42884537788346));
#6614=CARTESIAN_POINT('Ctrl Pts',(0.788798568359572,-3.5398689787538,4.57647137303824));
#6615=CARTESIAN_POINT('Ctrl Pts',(3.39559987896266,-1.27388265864876,4.73445453828687));
#6616=CARTESIAN_POINT('Ctrl Pts',(2.92247620064489,2.14755871250649,4.8924377035355));
#6617=CARTESIAN_POINT('Ctrl Pts',(-0.201433142800403,3.62109103191458,5.05042086878414));
#6618=CARTESIAN_POINT('Ctrl Pts',(-2.6783810755718,2.0960153254597,5.18346715187982));
#6619=CARTESIAN_POINT('Ctrl Pts',(-3.06794805030265,0.53695514470911,5.26385237989262));
#6620=CARTESIAN_POINT('Ctrl Pts',(-3.06862971834531,-0.000432433695450388,
5.29157655282255));
#6621=CARTESIAN_POINT('Ctrl Pts',(-3.07007340747988,-0.00202528632500865,
4.20842344717746));
#6622=CARTESIAN_POINT('Ctrl Pts',(-3.0723295005003,-0.370662586915465,4.22746411868935));
#6623=CARTESIAN_POINT('Ctrl Pts',(-2.84084702177449,-1.75610719556142,4.29916584528412));
#6624=CARTESIAN_POINT('Ctrl Pts',(-0.788798652099944,-3.53986935455429,
4.42352862696176));
#6625=CARTESIAN_POINT('Ctrl Pts',(2.53347023630324,-2.59507358691089,4.5815117922104));
#6626=CARTESIAN_POINT('Ctrl Pts',(3.55779514749501,0.703542499198116,4.73949495745903));
#6627=CARTESIAN_POINT('Ctrl Pts',(1.35507842480211,3.36402152542208,4.89747812270768));
#6628=CARTESIAN_POINT('Ctrl Pts',(-2.04038409747331,2.97735836442599,5.05378761928047));
#6629=CARTESIAN_POINT('Ctrl Pts',(-3.07571786407773,0.979775225389444,5.1574360607704));
#6630=CARTESIAN_POINT('Ctrl Pts',(-3.07829446204158,-0.000583257813248778,
5.20842344717746));
#6631=CARTESIAN_POINT('Origin',(0.,0.,-2.20842344717745));
#6632=CARTESIAN_POINT('',(-3.07132633130557,0.00250471562149607,3.20842344717745));
#6633=CARTESIAN_POINT('',(-3.07641449414843,-0.00211863766902523,3.29157655282255));
#6634=CARTESIAN_POINT('',(-3.0735,-1.43456032168185E-13,-2.20842344717745));
#6635=CARTESIAN_POINT('Ctrl Pts',(-3.07641449414843,-0.00211863766902543,
3.29157655282255));
#6636=CARTESIAN_POINT('Ctrl Pts',(-3.07748039759417,-0.137117714402335,
3.29858638556475));
#6637=CARTESIAN_POINT('Ctrl Pts',(-3.00831480734457,-1.28519241705506,3.35825727338983));
#6638=CARTESIAN_POINT('Ctrl Pts',(-1.56449671262057,-3.27188410457269,3.47058921629779));
#6639=CARTESIAN_POINT('Ctrl Pts',(1.88513481412996,-3.09824826393655,3.62857238154643));
#6640=CARTESIAN_POINT('Ctrl Pts',(3.6248847206042,-0.114395495228309,3.78655554679506));
#6641=CARTESIAN_POINT('Ctrl Pts',(2.07674046049821,2.97321789072832,3.9445387120437));
#6642=CARTESIAN_POINT('Ctrl Pts',(-1.35507828094373,3.36402116829015,4.10252187729233));
#6643=CARTESIAN_POINT('Ctrl Pts',(-2.96796315791591,1.41595115878974,4.21820115755195));
#6644=CARTESIAN_POINT('Ctrl Pts',(-3.07640391873074,0.202401789536568,4.28121938272868));
#6645=CARTESIAN_POINT('Ctrl Pts',(-3.07459996860257,0.00263219671087611,
4.29157655282254));
#6646=CARTESIAN_POINT('Ctrl Pts',(-3.07132633130557,0.00250471562149589,
3.20842344717745));
#6647=CARTESIAN_POINT('Ctrl Pts',(-3.06584026152828,-0.701641494300131,
3.24483112152541));
#6648=CARTESIAN_POINT('Ctrl Pts',(-2.47675782003803,-2.4325802671815,3.33389985095624));
#6649=CARTESIAN_POINT('Ctrl Pts',(0.39131691802336,-3.60551653188198,3.47562963546996));
#6650=CARTESIAN_POINT('Ctrl Pts',(3.23336081192176,-1.64263697190919,3.63361280071859));
#6651=CARTESIAN_POINT('Ctrl Pts',(3.14263608255428,1.81017037953698,3.79159596596722));
#6652=CARTESIAN_POINT('Ctrl Pts',(0.20143316418192,3.62109141633224,3.94957913121586));
#6653=CARTESIAN_POINT('Ctrl Pts',(-2.54597223044503,2.32515411521603,4.0885216249526));
#6654=CARTESIAN_POINT('Ctrl Pts',(-3.06608979205588,0.648882820391893,4.17480306360647));
#6655=CARTESIAN_POINT('Ctrl Pts',(-3.07007340747988,-0.00202528632500865,
4.20842344717746));
#6656=CARTESIAN_POINT('Origin',(0.,0.,-2.20842344717745));
#6657=CARTESIAN_POINT('',(-3.07837144959354,-0.000390310105172764,2.20842344717746));
#6658=CARTESIAN_POINT('',(-3.0686847313066,-0.00060378848225347,2.29157655282255));
#6659=CARTESIAN_POINT('',(-3.0735,-1.43456032168185E-13,-2.20842344717745));
#6660=CARTESIAN_POINT('Ctrl Pts',(-3.0686847313066,-0.000603788482253509,
2.29157655282255));
#6661=CARTESIAN_POINT('Ctrl Pts',(-3.06952252124188,-0.473087586699036,
2.31595338840081));
#6662=CARTESIAN_POINT('Ctrl Pts',(-2.7454388394421,-1.96518478392561,2.39299127906196));
#6663=CARTESIAN_POINT('Ctrl Pts',(-0.429356469436753,-3.60118425699533,
2.52269022480598));
#6664=CARTESIAN_POINT('Ctrl Pts',(2.78124872844843,-2.32755908045191,2.68067339005463));
#6665=CARTESIAN_POINT('Ctrl Pts',(3.46916639160829,1.05724176501438,2.83865655530325));
#6666=CARTESIAN_POINT('Ctrl Pts',(1.01043173169663,3.48308817136713,2.99663972055189));
#6667=CARTESIAN_POINT('Ctrl Pts',(-2.21503745439621,2.78219775503983,3.14761305305832));
#6668=CARTESIAN_POINT('Ctrl Pts',(-3.06947284561207,0.877056814069305,3.24592533048187));
#6669=CARTESIAN_POINT('Ctrl Pts',(-3.07641449414843,-0.00211863766902543,
3.29157655282255));
#6670=CARTESIAN_POINT('Ctrl Pts',(-3.07837144959354,-0.000390310105173098,
2.20842344717746));
#6671=CARTESIAN_POINT('Ctrl Pts',(-3.07841005815743,-0.021801014405184,
2.2095370692786));
#6672=CARTESIAN_POINT('Ctrl Pts',(-3.06854699220857,-1.05564638938531,2.26331174646262));
#6673=CARTESIAN_POINT('Ctrl Pts',(-1.9177361559176,-3.07817520619115,2.36974747872952));
#6674=CARTESIAN_POINT('Ctrl Pts',(1.52987013245233,-3.28821788231848,2.52773064397815));
#6675=CARTESIAN_POINT('Ctrl Pts',(3.58983249342927,-0.515733880008737,2.68571380922678));
#6676=CARTESIAN_POINT('Ctrl Pts',(2.39369399271082,2.72453792342614,2.84369697447542));
#6677=CARTESIAN_POINT('Ctrl Pts',(-0.973606524696896,3.49356106124283,3.00168013972405));
#6678=CARTESIAN_POINT('Ctrl Pts',(-2.88532029877192,1.64683564550024,3.12325563062473));
#6679=CARTESIAN_POINT('Ctrl Pts',(-3.073775462771,0.31685482580784,3.19217006644253));
#6680=CARTESIAN_POINT('Ctrl Pts',(-3.07132633130557,0.00250471562149589,
3.20842344717745));
#6681=CARTESIAN_POINT('Origin',(0.,0.,-2.20842344717745));
#6682=CARTESIAN_POINT('',(-3.07029648698129,-0.00213295581009409,1.20842344717745));
#6683=CARTESIAN_POINT('',(-3.07427865213087,0.00268124138861234,1.29157655282254));
#6684=CARTESIAN_POINT('',(-3.0735,-1.43456032168185E-13,-2.20842344717745));
#6685=CARTESIAN_POINT('Ctrl Pts',(-3.07427865213087,0.00268124138861233,
1.29157655282254));
#6686=CARTESIAN_POINT('Ctrl Pts',(-3.06696859167679,-0.802693165681438,
1.33332039123688));
#6687=CARTESIAN_POINT('Ctrl Pts',(-2.33184421030331,-2.63589937589878,1.42772528473409));
#6688=CARTESIAN_POINT('Ctrl Pts',(0.751386011701174,-3.5479949524756,1.57479123331418));
#6689=CARTESIAN_POINT('Ctrl Pts',(3.3819631285828,-1.30965902445964,1.73277439856281));
#6690=CARTESIAN_POINT('Ctrl Pts',(2.94498385958509,2.11658913035191,1.89075756381145));
#6691=CARTESIAN_POINT('Ctrl Pts',(-0.163196082436613,3.62301515147438,2.04874072906008));
#6692=CARTESIAN_POINT('Ctrl Pts',(-2.6665990793913,2.11786358985906,2.18234705873045));
#6693=CARTESIAN_POINT('Ctrl Pts',(-3.06771265130252,0.54761484384293,2.26329233331794));
#6694=CARTESIAN_POINT('Ctrl Pts',(-3.0686847313066,-0.000603788482253509,
2.29157655282255));
#6695=CARTESIAN_POINT('Ctrl Pts',(-3.07029648698129,-0.0021329558100943,
1.20842344717745));
#6696=CARTESIAN_POINT('Ctrl Pts',(-3.07262562444356,-0.359867988536013,
1.22690407211466));
#6697=CARTESIAN_POINT('Ctrl Pts',(-2.8500883529908,-1.73417835702742,1.29804575213475));
#6698=CARTESIAN_POINT('Ctrl Pts',(-0.82610974606013,-3.53132320122762,1.42184848723771));
#6699=CARTESIAN_POINT('Ctrl Pts',(2.50592737524966,-2.62168489533313,1.57983165248634));
#6700=CARTESIAN_POINT('Ctrl Pts',(3.56502744730094,0.665951678041991,1.73781481773498));
#6701=CARTESIAN_POINT('Ctrl Pts',(1.3905130838547,3.34952614641417,1.89579798298361));
#6702=CARTESIAN_POINT('Ctrl Pts',(-2.02101881154259,2.99747636377196,2.0526675261311));
#6703=CARTESIAN_POINT('Ctrl Pts',(-3.07658433315844,0.990670161723115,2.15687601419572));
#6704=CARTESIAN_POINT('Ctrl Pts',(-3.07837144959354,-0.000390310105173098,
2.20842344717746));
#6705=CARTESIAN_POINT('Origin',(0.,0.,-2.20842344717745));
#6706=CARTESIAN_POINT('',(-3.07033931526091,0.00363009148700105,0.208423447177454));
#6707=CARTESIAN_POINT('',(-3.0766916133949,-0.00189804245167501,0.291576552822545));
#6708=CARTESIAN_POINT('',(-3.0735,-1.43456032168185E-13,-2.20842344717745));
#6709=CARTESIAN_POINT('',(-0.793799282532864,2.9692229537457,0.));
#6710=CARTESIAN_POINT('Ctrl Pts',(-0.793799282532843,2.9692229537457,-1.11022302462516E-15));
#6711=CARTESIAN_POINT('Ctrl Pts',(-1.77625330176029,2.70657130793364,0.0526610550828771));
#6712=CARTESIAN_POINT('Ctrl Pts',(-2.87604924152809,1.66965640541239,0.122135537475362));
#6713=CARTESIAN_POINT('Ctrl Pts',(-3.07270725204059,0.328982361216722,0.191610019867847));
#6714=CARTESIAN_POINT('Ctrl Pts',(-3.07033931526091,0.00363009148700071,
0.208423447177454));
#6715=CARTESIAN_POINT('',(0.795570175323944,2.97434157986908,-1.73204294965629E-16));
#6716=CARTESIAN_POINT('Origin',(0.,0.,0.));
#6717=CARTESIAN_POINT('Ctrl Pts',(0.795572458610595,2.9743481795293,-4.90601483049691E-17));
#6718=CARTESIAN_POINT('Ctrl Pts',(-0.152115296302603,3.22551568492474,0.0509809153588237));
#6719=CARTESIAN_POINT('Ctrl Pts',(-2.21229639614352,2.76930588931089,0.148173099633005));
#6720=CARTESIAN_POINT('Ctrl Pts',(-3.06995895786669,0.887635565040844,0.245365283907187));
#6721=CARTESIAN_POINT('Ctrl Pts',(-3.0766916133949,-0.00189804245167461,
0.291576552822545));
#6722=CARTESIAN_POINT('Origin',(0.,0.,-2.20842344717745));
#6723=CARTESIAN_POINT('Ctrl Pts',(-3.0766916133949,-0.00189804245167473,
0.291576552822545));
#6724=CARTESIAN_POINT('Ctrl Pts',(-3.07763130168989,-0.126051775768505,
0.298026338990065));
#6725=CARTESIAN_POINT('Ctrl Pts',(-3.01464226329898,-1.26297686345005,0.357137180240463));
#6726=CARTESIAN_POINT('Ctrl Pts',(-1.59892885671069,-3.25553203106243,0.46890907657374));
#6727=CARTESIAN_POINT('Ctrl Pts',(1.85231282140687,-3.11779525816486,0.626892241822374));
#6728=CARTESIAN_POINT('Ctrl Pts',(3.62348061843826,-0.15274939435253,0.784875407071009));
#6729=CARTESIAN_POINT('Ctrl Pts',(2.10800845124216,2.95117859561544,0.942858572319642));
#6730=CARTESIAN_POINT('Ctrl Pts',(-1.31948921168312,3.3781127260263,1.10084173756828));
#6731=CARTESIAN_POINT('Ctrl Pts',(-2.96075827138585,1.43785809058675,1.21708106440258));
#6732=CARTESIAN_POINT('Ctrl Pts',(-3.07619044359204,0.213309857138166,1.280659336154));
#6733=CARTESIAN_POINT('Ctrl Pts',(-3.07427865213087,0.00268124138861233,
1.29157655282254));
#6734=CARTESIAN_POINT('Ctrl Pts',(-3.07033931526091,0.00363009148700071,
0.208423447177454));
#6735=CARTESIAN_POINT('Ctrl Pts',(-3.06529067677062,-0.690048053110911,
0.244271074950725));
#6736=CARTESIAN_POINT('Ctrl Pts',(-2.49208243053968,-2.41283008884042,0.332779757806875));
#6737=CARTESIAN_POINT('Ctrl Pts',(0.353891905593742,-3.60835904048448,0.473949495745902));
#6738=CARTESIAN_POINT('Ctrl Pts',(3.21549712367075,-1.67724424006994,0.631932660994537));
#6739=CARTESIAN_POINT('Ctrl Pts',(3.16174910309101,1.77718997587638,0.789915826243172));
#6740=CARTESIAN_POINT('Ctrl Pts',(0.239554143273228,3.61860888141612,0.947898991491804));
#6741=CARTESIAN_POINT('Ctrl Pts',(-2.53238151228791,2.3468476466272,1.08740153180324));
#6742=CARTESIAN_POINT('Ctrl Pts',(-3.06598868242385,0.659507943147289,1.17424301703178));
#6743=CARTESIAN_POINT('Ctrl Pts',(-3.07029648698129,-0.0021329558100943,
1.20842344717745));
#6744=CARTESIAN_POINT('Ctrl Pts',(1.91346599666506,-1.63598720337495,-2.77555756156289E-16));
#6745=CARTESIAN_POINT('Ctrl Pts',(2.45478008065218,-1.00286116724919,0.0526610550828779));
#6746=CARTESIAN_POINT('Ctrl Pts',(2.85088904111311,0.831797344758419,0.157983165248634));
#6747=CARTESIAN_POINT('Ctrl Pts',(0.857588690962395,2.84611954060091,0.315966330497269));
#6748=CARTESIAN_POINT('Ctrl Pts',(-1.91305892034906,2.27152017519409,0.473949495745902));
#6749=CARTESIAN_POINT('Ctrl Pts',(-2.94872155070904,-0.359723249961514,
0.631932660994538));
#6750=CARTESIAN_POINT('Ctrl Pts',(-1.30968062364378,-2.66660220862199,0.789915826243172));
#6751=CARTESIAN_POINT('Ctrl Pts',(1.51722711172663,-2.55378219047666,0.947898991491806));
#6752=CARTESIAN_POINT('Ctrl Pts',(2.96798843563309,-0.125116837573611,1.10588215674044));
#6753=CARTESIAN_POINT('Ctrl Pts',(1.72666708182923,2.41730669089373,1.26386532198907));
#6754=CARTESIAN_POINT('Ctrl Pts',(-1.08079196043997,2.76700790231697,1.42184848723771));
#6755=CARTESIAN_POINT('Ctrl Pts',(-2.90794013715773,0.607013050434708,1.57983165248634));
#6756=CARTESIAN_POINT('Ctrl Pts',(-2.09748509105245,-2.10360231788684,1.73781481773498));
#6757=CARTESIAN_POINT('Ctrl Pts',(0.615459340965577,-2.90615822119971,1.89579798298361));
#6758=CARTESIAN_POINT('Ctrl Pts',(2.77016176222782,-1.07274006639895,2.05378114823225));
#6759=CARTESIAN_POINT('Ctrl Pts',(2.41223259037106,1.7336955053395,2.21176431348088));
#6760=CARTESIAN_POINT('Ctrl Pts',(-0.133673706697308,2.96760717222605,2.36974747872952));
#6761=CARTESIAN_POINT('Ctrl Pts',(-2.55833347750605,1.50979936227371,2.52773064397815));
#6762=CARTESIAN_POINT('Ctrl Pts',(-2.66249741667059,-1.31744879591152,2.68571380922678));
#6763=CARTESIAN_POINT('Ctrl Pts',(-0.351685346285025,-2.94972551390458,
2.84369697447542));
#6764=CARTESIAN_POINT('Ctrl Pts',(2.27811734955878,-1.90650072719625,3.00168013972405));
#6765=CARTESIAN_POINT('Ctrl Pts',(2.84158984573739,0.865985405376183,3.15966330497269));
#6766=CARTESIAN_POINT('Ctrl Pts',(0.827643365721903,2.85299315809883,3.31764647022132));
#6767=CARTESIAN_POINT('Ctrl Pts',(-1.93700389804496,2.25223876861204,3.47562963546996));
#6768=CARTESIAN_POINT('Ctrl Pts',(-2.94472251124898,-0.391373073923526,
3.63361280071859));
#6769=CARTESIAN_POINT('Ctrl Pts',(-1.28147729755077,-2.67999617155092,3.79159596596722));
#6770=CARTESIAN_POINT('Ctrl Pts',(1.54411156485185,-2.53777127198967,3.94957913121586));
#6771=CARTESIAN_POINT('Ctrl Pts',(2.96913853395838,-0.0937012068447269,
4.10756229646449));
#6772=CARTESIAN_POINT('Ctrl Pts',(1.70105550977851,2.4353590499133,4.26554546171313));
#6773=CARTESIAN_POINT('Ctrl Pts',(-1.10994292249092,2.75546552502699,4.42352862696176));
#6774=CARTESIAN_POINT('Ctrl Pts',(-2.91418523928623,0.576270718626006,4.5815117922104));
#6775=CARTESIAN_POINT('Ctrl Pts',(-2.07516207671643,-2.12562129867421,4.73949495745903));
#6776=CARTESIAN_POINT('Ctrl Pts',(0.646103919259875,-2.89950224630314,4.89747812270767));
#6777=CARTESIAN_POINT('Ctrl Pts',(2.78133160738197,-1.04343568997828,5.0554612879563));
#6778=CARTESIAN_POINT('Ctrl Pts',(2.39379659512723,1.75906265128847,5.21344445320494));
#6779=CARTESIAN_POINT('Ctrl Pts',(-0.16499363494388,2.96603112830485,5.37142761845357));
#6780=CARTESIAN_POINT('Ctrl Pts',(-2.57412900533635,1.48270813296201,5.5294107837022));
#6781=CARTESIAN_POINT('Ctrl Pts',(-2.64844150963962,-1.34548174319338,5.68739394895084));
#6782=CARTESIAN_POINT('Ctrl Pts',(-0.320527163328734,-2.953273761345,5.84537711419947));
#6783=CARTESIAN_POINT('Ctrl Pts',(2.29811625201049,-1.8823456625252,6.00336027944811));
#6784=CARTESIAN_POINT('Ctrl Pts',(2.83228980319549,0.895934174165315,6.16134344469674));
#6785=CARTESIAN_POINT('Ctrl Pts',(0.797479800043391,2.8615711854999,6.31932660994538));
#6786=CARTESIAN_POINT('Ctrl Pts',(-1.9606715426706,2.23166536289225,6.47730977519401));
#6787=CARTESIAN_POINT('Ctrl Pts',(-2.94042698671483,-0.422436929523689,
6.63529294044265));
#6788=CARTESIAN_POINT('Ctrl Pts',(-1.25311457556089,-2.69337486380324,6.79327610569128));
#6789=CARTESIAN_POINT('Ctrl Pts',(1.57081511540494,-2.52132918551407,6.95125927093992));
#6790=CARTESIAN_POINT('Ctrl Pts',(2.96996266917328,-0.0623531795483424,
7.10924243618854));
#6791=CARTESIAN_POINT('Ctrl Pts',(1.67525120350748,2.45318177967176,7.26722560143719));
#6792=CARTESIAN_POINT('Ctrl Pts',(-1.13896739958789,2.74359236580518,7.42520876668581));
#6793=CARTESIAN_POINT('Ctrl Pts',(-2.92010921422275,0.545480151808999,7.58319193193445));
#6794=CARTESIAN_POINT('Ctrl Pts',(-2.0526017431469,-2.14741862912689,7.74117509718308));
#6795=CARTESIAN_POINT('Ctrl Pts',(0.67666536543526,-2.89250202704452,7.89915826243172));
#6796=CARTESIAN_POINT('Ctrl Pts',(2.79221254834523,-1.01405124829845,8.05714142768035));
#6797=CARTESIAN_POINT('Ctrl Pts',(2.37505367965917,1.78430087032248,8.21512459292899));
#6798=CARTESIAN_POINT('Ctrl Pts',(-0.196218413907403,2.96399728727909,8.37310775817763));
#6799=CARTESIAN_POINT('Ctrl Pts',(-2.58978452475258,1.45569460750793,8.53109092342626));
#6800=CARTESIAN_POINT('Ctrl Pts',(-2.63380935188005,-1.37382964669131,8.68907408867489));
#6801=CARTESIAN_POINT('Ctrl Pts',(-0.28987227158717,-2.95560017681787,8.84705725392352));
#6802=CARTESIAN_POINT('Ctrl Pts',(2.3189007506055,-1.85971882581699,9.00504041917216));
#6803=CARTESIAN_POINT('Ctrl Pts',(2.82058775165227,0.929376071735854,9.16302358442079));
#6804=CARTESIAN_POINT('Ctrl Pts',(1.45492685445962,2.21694916795929,9.26834569458655));
#6805=CARTESIAN_POINT('Ctrl Pts',(0.65019999797512,2.43208680203507,9.32100674966943));
#6806=CARTESIAN_POINT('Ctrl Pts',(2.05433155034209,-1.75642532122685,-0.107002249889811));
#6807=CARTESIAN_POINT('Ctrl Pts',(2.63549609850622,-1.07668980796293,-0.0543411948069327));
#6808=CARTESIAN_POINT('Ctrl Pts',(3.06076581130297,0.89303260774229,0.0509809153588233));
#6809=CARTESIAN_POINT('Ctrl Pts',(0.920722661458932,3.05564518966732,0.208964080607458));
#6810=CARTESIAN_POINT('Ctrl Pts',(-2.05389450587889,2.43874496399355,0.366947245856092));
#6811=CARTESIAN_POINT('Ctrl Pts',(-3.16580055530278,-0.386205358796813,
0.524930411104728));
#6812=CARTESIAN_POINT('Ctrl Pts',(-1.40609670133275,-2.86291214943547,0.682913576353361));
#6813=CARTESIAN_POINT('Ctrl Pts',(1.62892234828671,-2.74178654637273,0.840896741601996));
#6814=CARTESIAN_POINT('Ctrl Pts',(3.18648582990148,-0.13432768983325,0.99887990685063));
#6815=CARTESIAN_POINT('Ctrl Pts',(1.85378087163354,2.59526399246763,1.15686307209926));
#6816=CARTESIAN_POINT('Ctrl Pts',(-1.16035771085436,2.97070951022008,1.3148462373479));
#6817=CARTESIAN_POINT('Ctrl Pts',(-3.12201689535166,0.651700141602095,1.47282940259653));
#6818=CARTESIAN_POINT('Ctrl Pts',(-2.25189776376018,-2.25846532864422,1.63081256784517));
#6819=CARTESIAN_POINT('Ctrl Pts',(0.660768231210779,-3.12010379829167,1.7887957330938));
#6820=CARTESIAN_POINT('Ctrl Pts',(2.97409555101281,-1.15171305241918,1.94677889834243));
#6821=CARTESIAN_POINT('Ctrl Pts',(2.58981634677574,1.86132671367697,2.10476206359107));
#6822=CARTESIAN_POINT('Ctrl Pts',(-0.143514498610412,3.18607649864216,2.26274522883971));
#6823=CARTESIAN_POINT('Ctrl Pts',(-2.74667289008379,1.62094778272047,2.42072839408834));
#6824=CARTESIAN_POINT('Ctrl Pts',(-2.8585051708803,-1.41443675096306,2.57871155933698));
#6825=CARTESIAN_POINT('Ctrl Pts',(-0.377575720668934,-3.16687842826817,
2.7366947245856));
#6826=CARTESIAN_POINT('Ctrl Pts',(2.44582780918866,-2.0468535116148,2.89467788983425));
#6827=CARTESIAN_POINT('Ctrl Pts',(3.05078202769436,0.92973752525558,3.05266105508288));
#6828=CARTESIAN_POINT('Ctrl Pts',(0.888572821046812,3.06302482918826,3.21064422033151));
#6829=CARTESIAN_POINT('Ctrl Pts',(-2.07960226511719,2.41804409868132,3.36862738558015));
#6830=CARTESIAN_POINT('Ctrl Pts',(-3.16150711452663,-0.420185179729744,
3.52661055082878));
#6831=CARTESIAN_POINT('Ctrl Pts',(-1.37581710257403,-2.87729214922485,3.68459371607741));
#6832=CARTESIAN_POINT('Ctrl Pts',(1.65778598127789,-2.72459693597196,3.84257688132606));
#6833=CARTESIAN_POINT('Ctrl Pts',(3.18772059617366,-0.100599302972588,4.00056004657468));
#6834=CARTESIAN_POINT('Ctrl Pts',(1.82628382668507,2.61464533018498,4.15854321182332));
#6835=CARTESIAN_POINT('Ctrl Pts',(-1.19165470864185,2.95831740611471,4.31652637707195));
#6836=CARTESIAN_POINT('Ctrl Pts',(-3.12872174945414,0.618694620586424,4.47450954232059));
#6837=CARTESIAN_POINT('Ctrl Pts',(-2.22793137359221,-2.28210530291954,4.63249270756923));
#6838=CARTESIAN_POINT('Ctrl Pts',(0.693668802293106,-3.1129578237867,4.79047587281786));
#6839=CARTESIAN_POINT('Ctrl Pts',(2.98608769790887,-1.12025134620178,4.94845903806649));
#6840=CARTESIAN_POINT('Ctrl Pts',(2.57002313029978,1.88856133836114,5.10644220331513));
#6841=CARTESIAN_POINT('Ctrl Pts',(-0.177140137562721,3.18438442950809,5.26442536856376));
#6842=CARTESIAN_POINT('Ctrl Pts',(-2.76363125319693,1.59186215109202,5.42240853381239));
#6843=CARTESIAN_POINT('Ctrl Pts',(-2.84341449598317,-1.44453342796206,5.58039169906103));
#6844=CARTESIAN_POINT('Ctrl Pts',(-0.34412373437286,-3.1706878906145,5.73837486430966));
#6845=CARTESIAN_POINT('Ctrl Pts',(2.4672989909867,-2.0209201992169,5.89635802955829));
#6846=CARTESIAN_POINT('Ctrl Pts',(3.04079733455288,0.961891062723529,6.05434119480694));
#6847=CARTESIAN_POINT('Ctrl Pts',(0.856188673770513,3.07223435387301,6.21232436005557));
#6848=CARTESIAN_POINT('Ctrl Pts',(-2.10501227457723,2.39595611982943,6.3703075253042));
#6849=CARTESIAN_POINT('Ctrl Pts',(-3.15689536203605,-0.453535894477701,
6.52829069055284));
#6850=CARTESIAN_POINT('Ctrl Pts',(-1.34536637351016,-2.89165575414083,6.68627385580147));
#6851=CARTESIAN_POINT('Ctrl Pts',(1.68645539401005,-2.70694441585446,6.8442570210501));
#6852=CARTESIAN_POINT('Ctrl Pts',(3.18860540258081,-0.0669434963744089,
7.00224018629874));
#6853=CARTESIAN_POINT('Ctrl Pts',(1.79857985880707,2.63378013379257,7.16022335154736));
#6854=CARTESIAN_POINT('Ctrl Pts',(-1.22281590990512,2.94557016857085,7.31820651679601));
#6855=CARTESIAN_POINT('Ctrl Pts',(-3.13508183562068,0.585637313597254,7.47618968204465));
#6856=CARTESIAN_POINT('Ctrl Pts',(-2.20371019322167,-2.30550730940422,7.63417284729327));
#6857=CARTESIAN_POINT('Ctrl Pts',(0.726480121235595,-3.10544226233571,7.79215601254191));
#6858=CARTESIAN_POINT('Ctrl Pts',(2.9977696720632,-1.08870368048037,7.95013917779055));
#6859=CARTESIAN_POINT('Ctrl Pts',(2.54990039874432,1.9156575447878,8.10812234303918));
#6860=CARTESIAN_POINT('Ctrl Pts',(-0.210663622531375,3.18220086115888,8.26610550828781));
#6861=CARTESIAN_POINT('Ctrl Pts',(-2.78043930075555,1.56285994372434,8.42408867353645));
#6862=CARTESIAN_POINT('Ctrl Pts',(-2.8277051479271,-1.47496824762615,8.58207183878509));
#6863=CARTESIAN_POINT('Ctrl Pts',(-0.311212090587828,-3.17318557215857,
8.74005500403371));
#6864=CARTESIAN_POINT('Ctrl Pts',(2.48961360295064,-1.99662761987913,8.89803816928235));
#6865=CARTESIAN_POINT('Ctrl Pts',(3.02823380129393,0.997794886152954,9.05602133453098));
#6866=CARTESIAN_POINT('Ctrl Pts',(1.56203567022653,2.38015654795073,9.16134344469674));
#6867=CARTESIAN_POINT('Ctrl Pts',(0.69806642616104,2.61113218593861,9.21400449977962));
#6868=CARTESIAN_POINT('Ctrl Pts',(2.19519710401912,-1.87686343907875,-0.214004499779622));
#6869=CARTESIAN_POINT('Ctrl Pts',(2.81621211636026,-1.15051844867667,-0.161343444696743));
#6870=CARTESIAN_POINT('Ctrl Pts',(3.27064258149282,0.954267870726162,-0.0560213345309874));
#6871=CARTESIAN_POINT('Ctrl Pts',(0.983856631955468,3.26517083873374,0.101961830717648));
#6872=CARTESIAN_POINT('Ctrl Pts',(-2.19473009140873,2.60596975279301,0.259944995966281));
#6873=CARTESIAN_POINT('Ctrl Pts',(-3.38287955989652,-0.412687467632114,
0.417928161214917));
#6874=CARTESIAN_POINT('Ctrl Pts',(-1.50251277902172,-3.05922209024895,0.57591132646355));
#6875=CARTESIAN_POINT('Ctrl Pts',(1.74061758484679,-2.92979090226879,0.733894491712185));
#6876=CARTESIAN_POINT('Ctrl Pts',(3.40498322416987,-0.14353854209289,0.891877656960819));
#6877=CARTESIAN_POINT('Ctrl Pts',(1.98089466143785,2.77322129404153,1.04986082220945));
#6878=CARTESIAN_POINT('Ctrl Pts',(-1.23992346126874,3.17441111812319,1.20784398745809));
#6879=CARTESIAN_POINT('Ctrl Pts',(-3.3360936535456,0.696387232769482,1.36582715270672));
#6880=CARTESIAN_POINT('Ctrl Pts',(-2.40631043646792,-2.41332833940159,1.52381031795536));
#6881=CARTESIAN_POINT('Ctrl Pts',(0.706077121455976,-3.33404937538364,1.68179348320399));
#6882=CARTESIAN_POINT('Ctrl Pts',(3.1780293397978,-1.23068603843941,1.83977664845263));
#6883=CARTESIAN_POINT('Ctrl Pts',(2.76740010318042,1.98895792201444,1.99775981370126));
#6884=CARTESIAN_POINT('Ctrl Pts',(-0.153355290523512,3.40454582505827,2.1557429789499));
#6885=CARTESIAN_POINT('Ctrl Pts',(-2.93501230266153,1.73209620316724,2.31372614419853));
#6886=CARTESIAN_POINT('Ctrl Pts',(-3.05451292509001,-1.51142470601461,2.47170930944717));
#6887=CARTESIAN_POINT('Ctrl Pts',(-0.403466095052845,-3.38403134263174,
2.62969247469579));
#6888=CARTESIAN_POINT('Ctrl Pts',(2.61353826881855,-2.18720629603336,2.78767563994443));
#6889=CARTESIAN_POINT('Ctrl Pts',(3.25997420965132,0.993489645134981,2.94565880519306));
#6890=CARTESIAN_POINT('Ctrl Pts',(0.949502276371721,3.27305650027769,3.1036419704417));
#6891=CARTESIAN_POINT('Ctrl Pts',(-2.22220063218942,2.58384942875061,3.26162513569034));
#6892=CARTESIAN_POINT('Ctrl Pts',(-3.37829171780428,-0.448997285535967,
3.41960830093897));
#6893=CARTESIAN_POINT('Ctrl Pts',(-1.4701569075973,-3.07458812689877,3.5775914661876));
#6894=CARTESIAN_POINT('Ctrl Pts',(1.77146039770392,-2.91142259995426,3.73557463143624));
#6895=CARTESIAN_POINT('Ctrl Pts',(3.40630265838893,-0.107497399100449,3.89355779668488));
#6896=CARTESIAN_POINT('Ctrl Pts',(1.95151214359164,2.79393161045665,4.0515409619335));
#6897=CARTESIAN_POINT('Ctrl Pts',(-1.27336649479279,3.16116928720243,4.20952412718215));
#6898=CARTESIAN_POINT('Ctrl Pts',(-3.34325825962205,0.661118522546843,4.36750729243077));
#6899=CARTESIAN_POINT('Ctrl Pts',(-2.38070067046799,-2.43858930716488,4.52549045767941));
#6900=CARTESIAN_POINT('Ctrl Pts',(0.741233685326339,-3.32641340127025,4.68347362292804));
#6901=CARTESIAN_POINT('Ctrl Pts',(3.19084378843576,-1.19706700242527,4.84145678817668));
#6902=CARTESIAN_POINT('Ctrl Pts',(2.74624966547234,2.01806002543382,4.99943995342531));
#6903=CARTESIAN_POINT('Ctrl Pts',(-0.18928664018156,3.40273773071133,5.15742311867395));
#6904=CARTESIAN_POINT('Ctrl Pts',(-2.95313350105751,1.70101616922202,5.31540628392258));
#6905=CARTESIAN_POINT('Ctrl Pts',(-3.03838748232671,-1.54358511273075,5.47338944917122));
#6906=CARTESIAN_POINT('Ctrl Pts',(-0.36772030541699,-3.38810201988398,5.63137261441986));
#6907=CARTESIAN_POINT('Ctrl Pts',(2.63648172996291,-2.15949473590859,5.78935577966849));
#6908=CARTESIAN_POINT('Ctrl Pts',(3.24930486591027,1.02784795128174,5.94733894491712));
#6909=CARTESIAN_POINT('Ctrl Pts',(0.914897547497642,3.28289752224612,6.10532211016575));
#6910=CARTESIAN_POINT('Ctrl Pts',(-2.24935300648386,2.56024687676662,6.26330527541439));
#6911=CARTESIAN_POINT('Ctrl Pts',(-3.37336373735726,-0.484634859431713,
6.42128844066303));
#6912=CARTESIAN_POINT('Ctrl Pts',(-1.43761817145943,-3.08993664447841,6.57927160591165));
#6913=CARTESIAN_POINT('Ctrl Pts',(1.80209567261517,-2.89255964619486,6.7372547711603));
#6914=CARTESIAN_POINT('Ctrl Pts',(3.40724813598833,-0.071533813200476,6.89523793640892));
#6915=CARTESIAN_POINT('Ctrl Pts',(1.92190851410666,2.81437848791339,7.05322110165757));
#6916=CARTESIAN_POINT('Ctrl Pts',(-1.30666442022235,3.14754797133651,7.2112042669062));
#6917=CARTESIAN_POINT('Ctrl Pts',(-3.35005445701861,0.62579447538551,7.36918743215483));
#6918=CARTESIAN_POINT('Ctrl Pts',(-2.35481864329643,-2.46359598968156,7.52717059740347));
#6919=CARTESIAN_POINT('Ctrl Pts',(0.776294877035925,-3.31838249762691,7.6851537626521));
#6920=CARTESIAN_POINT('Ctrl Pts',(3.20332679578117,-1.16335611266229,7.84313692790073));
#6921=CARTESIAN_POINT('Ctrl Pts',(2.72474711782945,2.04701421925312,8.00112009314937));
#6922=CARTESIAN_POINT('Ctrl Pts',(-0.225108831155339,3.40040443503868,8.15910325839799));
#6923=CARTESIAN_POINT('Ctrl Pts',(-2.97109407675852,1.67002527994074,8.31708642364664));
#6924=CARTESIAN_POINT('Ctrl Pts',(-3.02160094397414,-1.57610684856099,8.47506958889527));
#6925=CARTESIAN_POINT('Ctrl Pts',(-0.332551909588488,-3.39077096749929,
8.63305275414391));
#6926=CARTESIAN_POINT('Ctrl Pts',(2.66032645529578,-2.13353641394126,8.79103591939254));
#6927=CARTESIAN_POINT('Ctrl Pts',(3.2358798509356,1.06621370057005,8.94901908464117));
#6928=CARTESIAN_POINT('Ctrl Pts',(1.66914448599343,2.54336392794217,9.05434119480693));
#6929=CARTESIAN_POINT('Ctrl Pts',(0.745932854346961,2.79017756984215,9.10700224988981));
#6930=CARTESIAN_POINT('Ctrl Pts',(2.33606265769615,-1.99730155693065,-0.321006749669432));
#6931=CARTESIAN_POINT('Ctrl Pts',(2.99692813421429,-1.22434708939042,-0.268345694586554));
#6932=CARTESIAN_POINT('Ctrl Pts',(3.48051935168267,1.01550313371003,-0.163023584420798));
#6933=CARTESIAN_POINT('Ctrl Pts',(1.04699060245201,3.47469648780015,-0.00504041917216321));
#6934=CARTESIAN_POINT('Ctrl Pts',(-2.33556567693856,2.77319454159246,0.152942746076471));
#6935=CARTESIAN_POINT('Ctrl Pts',(-3.59995856449026,-0.439169576467412,
0.310925911325106));
#6936=CARTESIAN_POINT('Ctrl Pts',(-1.59892885671069,-3.25553203106243,0.46890907657374));
#6937=CARTESIAN_POINT('Ctrl Pts',(1.85231282140687,-3.11779525816486,0.626892241822374));
#6938=CARTESIAN_POINT('Ctrl Pts',(3.62348061843826,-0.15274939435253,0.784875407071009));
#6939=CARTESIAN_POINT('Ctrl Pts',(2.10800845124216,2.95117859561544,0.942858572319642));
#6940=CARTESIAN_POINT('Ctrl Pts',(-1.31948921168312,3.3781127260263,1.10084173756828));
#6941=CARTESIAN_POINT('Ctrl Pts',(-3.55017041173953,0.741074323936872,1.25882490281691));
#6942=CARTESIAN_POINT('Ctrl Pts',(-2.56072310917565,-2.56819135015897,1.41680806806555));
#6943=CARTESIAN_POINT('Ctrl Pts',(0.751386011701174,-3.5479949524756,1.57479123331418));
#6944=CARTESIAN_POINT('Ctrl Pts',(3.3819631285828,-1.30965902445964,1.73277439856281));
#6945=CARTESIAN_POINT('Ctrl Pts',(2.94498385958509,2.11658913035191,1.89075756381145));
#6946=CARTESIAN_POINT('Ctrl Pts',(-0.163196082436613,3.62301515147438,2.04874072906008));
#6947=CARTESIAN_POINT('Ctrl Pts',(-3.12335171523926,1.843244623614,2.20672389430872));
#6948=CARTESIAN_POINT('Ctrl Pts',(-3.25052067929972,-1.60841266106616,2.36470705955735));
#6949=CARTESIAN_POINT('Ctrl Pts',(-0.429356469436753,-3.60118425699533,
2.52269022480598));
#6950=CARTESIAN_POINT('Ctrl Pts',(2.78124872844843,-2.32755908045191,2.68067339005463));
#6951=CARTESIAN_POINT('Ctrl Pts',(3.46916639160829,1.05724176501438,2.83865655530325));
#6952=CARTESIAN_POINT('Ctrl Pts',(1.01043173169663,3.48308817136713,2.99663972055189));
#6953=CARTESIAN_POINT('Ctrl Pts',(-2.36479899926165,2.74965475881989,3.15462288580052));
#6954=CARTESIAN_POINT('Ctrl Pts',(-3.59507632108192,-0.477809391342187,
3.31260605104916));
#6955=CARTESIAN_POINT('Ctrl Pts',(-1.56449671262057,-3.27188410457269,3.47058921629779));
#6956=CARTESIAN_POINT('Ctrl Pts',(1.88513481412996,-3.09824826393655,3.62857238154643));
#6957=CARTESIAN_POINT('Ctrl Pts',(3.6248847206042,-0.114395495228309,3.78655554679506));
#6958=CARTESIAN_POINT('Ctrl Pts',(2.07674046049821,2.97321789072832,3.9445387120437));
#6959=CARTESIAN_POINT('Ctrl Pts',(-1.35507828094373,3.36402116829015,4.10252187729233));
#6960=CARTESIAN_POINT('Ctrl Pts',(-3.55779476978996,0.703542424507262,4.26050504254097));
#6961=CARTESIAN_POINT('Ctrl Pts',(-2.53346996734378,-2.59507331141021,4.4184882077896));
#6962=CARTESIAN_POINT('Ctrl Pts',(0.788798568359572,-3.5398689787538,4.57647137303824));
#6963=CARTESIAN_POINT('Ctrl Pts',(3.39559987896266,-1.27388265864876,4.73445453828687));
#6964=CARTESIAN_POINT('Ctrl Pts',(2.92247620064489,2.14755871250649,4.8924377035355));
#6965=CARTESIAN_POINT('Ctrl Pts',(-0.201433142800403,3.62109103191458,5.05042086878414));
#6966=CARTESIAN_POINT('Ctrl Pts',(-3.14263574891808,1.81017018735203,5.20840403403277));
#6967=CARTESIAN_POINT('Ctrl Pts',(-3.23336046867026,-1.64263679749944,5.36638719928141));
#6968=CARTESIAN_POINT('Ctrl Pts',(-0.391316876461119,-3.60551614915347,
5.52437036453005));
#6969=CARTESIAN_POINT('Ctrl Pts',(2.80566446893912,-2.29806927260028,5.68235352977867));
#6970=CARTESIAN_POINT('Ctrl Pts',(3.45781239726766,1.09380483983996,5.84033669502732));
#6971=CARTESIAN_POINT('Ctrl Pts',(0.97360642122477,3.49356069061924,5.99831986027594));
#6972=CARTESIAN_POINT('Ctrl Pts',(-2.3936937383905,2.7245376337038,6.15630302552459));
#6973=CARTESIAN_POINT('Ctrl Pts',(-3.58983211267847,-0.515733824385723,
6.31428619077321));
#6974=CARTESIAN_POINT('Ctrl Pts',(-1.5298699694087,-3.288217534816,6.47226935602186));
#6975=CARTESIAN_POINT('Ctrl Pts',(1.91773595122029,-3.07817487653525,6.63025252127048));
#6976=CARTESIAN_POINT('Ctrl Pts',(3.62589086939586,-0.0761241300265441,
6.78823568651912));
#6977=CARTESIAN_POINT('Ctrl Pts',(2.04523716940625,2.99497684203422,6.94621885176775));
#6978=CARTESIAN_POINT('Ctrl Pts',(-1.39051293053958,3.34952577410217,7.10420201701639));
#6979=CARTESIAN_POINT('Ctrl Pts',(-3.56502707841653,0.665951637173768,7.26218518226502));
#6980=CARTESIAN_POINT('Ctrl Pts',(-2.5059270933712,-2.62168466995889,7.42016834751365));
#6981=CARTESIAN_POINT('Ctrl Pts',(0.826109632836259,-3.5313227329181,7.57815151276229));
#6982=CARTESIAN_POINT('Ctrl Pts',(3.40888391949913,-1.23800854484421,7.73613467801092));
#6983=CARTESIAN_POINT('Ctrl Pts',(2.89959383691459,2.17837089371843,7.89411784325955));
#6984=CARTESIAN_POINT('Ctrl Pts',(-0.239554039779309,3.61860800891848,8.0521010085082));
#6985=CARTESIAN_POINT('Ctrl Pts',(-3.16174885276149,1.77719061615714,8.21008417375682));
#6986=CARTESIAN_POINT('Ctrl Pts',(-3.21549674002119,-1.67724544949582,8.36806733900547));
#6987=CARTESIAN_POINT('Ctrl Pts',(-0.353891728589143,-3.60835636284,8.52605050425409));
#6988=CARTESIAN_POINT('Ctrl Pts',(2.83103930764092,-2.27044520800339,8.68403366950274));
#6989=CARTESIAN_POINT('Ctrl Pts',(3.44352590057726,1.13463251498715,8.84201683475136));
#6990=CARTESIAN_POINT('Ctrl Pts',(1.77625330176034,2.70657130793361,8.94733894491712));
#6991=CARTESIAN_POINT('Ctrl Pts',(0.793799282532882,2.96922295374569,9.));
#6992=CARTESIAN_POINT('Ctrl Pts',(0.793799282532882,2.96922295374569,9.));
#6993=CARTESIAN_POINT('Ctrl Pts',(0.886878490836273,2.9351741635662,9.));
#6994=CARTESIAN_POINT('Ctrl Pts',(0.977892261281868,2.89636065937617,9.));
#6995=CARTESIAN_POINT('Ctrl Pts',(1.0666317018473,2.85310967040871,9.));
#6996=CARTESIAN_POINT('Ctrl Pts',(1.15732414289755,2.80890680252603,9.));
#6997=CARTESIAN_POINT('Ctrl Pts',(1.24564171258029,2.76006836197957,9.));
#6998=CARTESIAN_POINT('Ctrl Pts',(1.33133249020885,2.70689814911949,9.));
#6999=CARTESIAN_POINT('Ctrl Pts',(1.41378164632743,2.65573932780546,9.));
#7000=CARTESIAN_POINT('Ctrl Pts',(1.49379927546973,2.60056939696339,9.));
#7001=CARTESIAN_POINT('Ctrl Pts',(1.57112798504849,2.54162891700393,9.));
#7002=CARTESIAN_POINT('Ctrl Pts',(1.6387906059299,2.4900559970394,9.));
#7003=CARTESIAN_POINT('Ctrl Pts',(1.70439423245071,2.43559555361028,9.));
#7004=CARTESIAN_POINT('Ctrl Pts',(1.76774178614759,2.37839602731573,9.));
#7005=CARTESIAN_POINT('Ctrl Pts',(1.78181925285965,2.36568481148552,9.));
#7006=CARTESIAN_POINT('Ctrl Pts',(1.79578788660031,2.35283565182172,8.99999999999999));
#7007=CARTESIAN_POINT('Ctrl Pts',(1.80962611638746,2.33986853565167,8.99999999999999));
#7008=CARTESIAN_POINT('Ctrl Pts',(1.88206130473834,2.27199312697639,8.99999999999999));
#7009=CARTESIAN_POINT('Ctrl Pts',(1.95103093355494,2.20079709720709,9.));
#7010=CARTESIAN_POINT('Ctrl Pts',(2.01629483992911,2.12656978280043,9.));
#7011=CARTESIAN_POINT('Ctrl Pts',(2.0811938619788,2.05275746628435,9.));
#7012=CARTESIAN_POINT('Ctrl Pts',(2.14242896847189,1.97594687106671,9.));
#7013=CARTESIAN_POINT('Ctrl Pts',(2.19972040363224,1.89639573891051,9.));
#7014=CARTESIAN_POINT('Ctrl Pts',(2.25491851002233,1.81975126589425,9.));
#7015=CARTESIAN_POINT('Ctrl Pts',(2.30645603825338,1.74056213090656,9.));
#7016=CARTESIAN_POINT('Ctrl Pts',(2.35403785390585,1.65904519358341,9.));
#7017=CARTESIAN_POINT('Ctrl Pts',(2.37402534994049,1.62480271167807,9.));
#7018=CARTESIAN_POINT('Ctrl Pts',(2.3933142673739,1.59014936887301,9.));
#7019=CARTESIAN_POINT('Ctrl Pts',(2.41188012691626,1.55510093684168,9.));
#7020=CARTESIAN_POINT('Ctrl Pts',(2.42490948045064,1.53050426192231,9.));
#7021=CARTESIAN_POINT('Ctrl Pts',(2.43758268759006,1.50571299850418,8.99999999999999));
#7022=CARTESIAN_POINT('Ctrl Pts',(2.44989080186182,1.48073259132809,8.99999999999999));
#7023=CARTESIAN_POINT('Ctrl Pts',(2.45765276114193,1.46497900803983,8.99999999999999));
#7024=CARTESIAN_POINT('Ctrl Pts',(2.46527041180683,1.44914804972639,9.));
#7025=CARTESIAN_POINT('Ctrl Pts',(2.47273181388943,1.43326226638681,9.));
#7026=CARTESIAN_POINT('Ctrl Pts',(2.51485724445469,1.34357463722026,9.));
#7027=CARTESIAN_POINT('Ctrl Pts',(2.55207933717843,1.25199813943898,8.99999999999999));
#7028=CARTESIAN_POINT('Ctrl Pts',(2.58410618468256,1.15880393051645,8.99999999999999));
#7029=CARTESIAN_POINT('Ctrl Pts',(2.613967295916,1.07191174924295,8.99999999999999));
#7030=CARTESIAN_POINT('Ctrl Pts',(2.63931185864415,0.983612456000679,8.99999999999999));
#7031=CARTESIAN_POINT('Ctrl Pts',(2.65985272591902,0.894117096452653,8.99999999999999));
#7032=CARTESIAN_POINT('Ctrl Pts',(2.66134249302584,0.88762626814031,8.99999999999999));
#7033=CARTESIAN_POINT('Ctrl Pts',(2.66280696907164,0.881129147123167,9.));
#7034=CARTESIAN_POINT('Ctrl Pts',(2.66424603364624,0.874625813581576,9.));
#7035=CARTESIAN_POINT('Ctrl Pts',(2.68483036310423,0.781602357540593,9.));
#7036=CARTESIAN_POINT('Ctrl Pts',(2.70021964474849,0.687306813520904,8.99999999999999));
#7037=CARTESIAN_POINT('Ctrl Pts',(2.71049110049637,0.592148341441679,8.99999999999999));
#7038=CARTESIAN_POINT('Ctrl Pts',(2.71630602466642,0.538276785854983,8.99999999999999));
#7039=CARTESIAN_POINT('Ctrl Pts',(2.72047976538942,0.484128852777968,8.99999999999999));
#7040=CARTESIAN_POINT('Ctrl Pts',(2.72301944391314,0.429781474340432,8.99999999999999));
#7041=CARTESIAN_POINT('Ctrl Pts',(2.72366615629779,0.415942272890204,8.99999999999999));
#7042=CARTESIAN_POINT('Ctrl Pts',(2.72420675980841,0.402091536187543,8.99999999999999));
#7043=CARTESIAN_POINT('Ctrl Pts',(2.72464119129261,0.388242780953578,8.99999999999999));
#7044=CARTESIAN_POINT('Ctrl Pts',(2.72756592883874,0.295008344975862,8.99999999999999));
#7045=CARTESIAN_POINT('Ctrl Pts',(2.72569048952638,0.201712560084688,8.99999999999999));
#7046=CARTESIAN_POINT('Ctrl Pts',(2.71914995708096,0.108731817539428,8.99999999999999));
#7047=CARTESIAN_POINT('Ctrl Pts',(2.71259904187879,0.0156034728777771,8.99999999999999));
#7048=CARTESIAN_POINT('Ctrl Pts',(2.70136783128446,-0.0772098102983187,
9.));
#7049=CARTESIAN_POINT('Ctrl Pts',(2.68554114262277,-0.169317716284785,9.));
#7050=CARTESIAN_POINT('Ctrl Pts',(2.66994282533527,-0.26009655025162,9.));
#7051=CARTESIAN_POINT('Ctrl Pts',(2.64988023184904,-0.350191061744686,8.99999999999999));
#7052=CARTESIAN_POINT('Ctrl Pts',(2.62539158794444,-0.439202338063852,8.99999999999999));
#7053=CARTESIAN_POINT('Ctrl Pts',(2.61615142083263,-0.472788479919204,8.99999999999999));
#7054=CARTESIAN_POINT('Ctrl Pts',(2.60628069313125,-0.506220073097839,8.99999999999999));
#7055=CARTESIAN_POINT('Ctrl Pts',(2.59578003712001,-0.539474360311661,8.99999999999999));
#7056=CARTESIAN_POINT('Ctrl Pts',(2.58810284762471,-0.563787076031328,8.99999999999999));
#7057=CARTESIAN_POINT('Ctrl Pts',(2.58008892698161,-0.588005000779692,9.));
#7058=CARTESIAN_POINT('Ctrl Pts',(2.57173827761392,-0.612118947017522,9.));
#7059=CARTESIAN_POINT('Ctrl Pts',(2.56654744841136,-0.627108365302125,9.));
#7060=CARTESIAN_POINT('Ctrl Pts',(2.56122944831744,-0.642049055238963,9.));
#7061=CARTESIAN_POINT('Ctrl Pts',(2.55578559038208,-0.656936550189778,9.));
#7062=CARTESIAN_POINT('Ctrl Pts',(2.52407277337967,-0.74366261993773,9.));
#7063=CARTESIAN_POINT('Ctrl Pts',(2.48808278639107,-0.828614124972656,8.99999999999999));
#7064=CARTESIAN_POINT('Ctrl Pts',(2.44787615884381,-0.911389078637309,8.99999999999999));
#7065=CARTESIAN_POINT('Ctrl Pts',(2.41772118818337,-0.973470293885799,8.99999999999999));
#7066=CARTESIAN_POINT('Ctrl Pts',(2.38519336783533,-1.03432671407457,9.));
#7067=CARTESIAN_POINT('Ctrl Pts',(2.35030314291149,-1.09377373790908,9.));
#7068=CARTESIAN_POINT('Ctrl Pts',(2.33453824589156,-1.12063444777661,9.));
#7069=CARTESIAN_POINT('Ctrl Pts',(2.31829087129828,-1.14720721377719,8.99999999999999));
#7070=CARTESIAN_POINT('Ctrl Pts',(2.30156120509674,-1.17347393974025,8.99999999999999));
#7071=CARTESIAN_POINT('Ctrl Pts',(2.2924219311199,-1.18782322813365,8.99999999999999));
#7072=CARTESIAN_POINT('Ctrl Pts',(2.28314386923737,-1.2020730730672,8.99999999999999));
#7073=CARTESIAN_POINT('Ctrl Pts',(2.27372778298295,-1.21622031438468,8.99999999999999));
#7074=CARTESIAN_POINT('Ctrl Pts',(2.22615751395616,-1.2876924799188,9.));
#7075=CARTESIAN_POINT('Ctrl Pts',(2.1750638810293,-1.35655384480895,9.));
#7076=CARTESIAN_POINT('Ctrl Pts',(2.12047811064926,-1.42245018095699,9.));
#7077=CARTESIAN_POINT('Ctrl Pts',(2.07432912024645,-1.47816157539741,9.));
#7078=CARTESIAN_POINT('Ctrl Pts',(2.02568338366803,-1.53175330505423,9.));
#7079=CARTESIAN_POINT('Ctrl Pts',(1.9745434647085,-1.58298712738403,9.));
#7080=CARTESIAN_POINT('Ctrl Pts',(1.95571094048283,-1.60185423198313,9.));
#7081=CARTESIAN_POINT('Ctrl Pts',(1.93654003149783,-1.62040132784491,9.));
#7082=CARTESIAN_POINT('Ctrl Pts',(1.91704088636911,-1.63862413454171,9.));
#7083=CARTESIAN_POINT('Ctrl Pts',(1.91346599666506,-1.63598720337495,-2.77555756156289E-16));
#7084=CARTESIAN_POINT('Ctrl Pts',(1.97510134314003,-1.57806511239367,-2.79433823621938E-16));
#7085=CARTESIAN_POINT('Ctrl Pts',(2.03336881374227,-1.51699406877496,-6.96361421210227E-16));
#7086=CARTESIAN_POINT('Ctrl Pts',(2.08826993179399,-1.45315846421965,-6.07153216591882E-16));
#7087=CARTESIAN_POINT('Ctrl Pts',(2.14462172708504,-1.38763610242017,-5.15587822965493E-16));
#7088=CARTESIAN_POINT('Ctrl Pts',(2.19742735662698,-1.31920071895718,-2.3862995218317E-16));
#7089=CARTESIAN_POINT('Ctrl Pts',(2.24666298209029,-1.24821943486301,-1.59594559789866E-16));
#7090=CARTESIAN_POINT('Ctrl Pts',(2.29723880045605,-1.1753060414018,-7.84078253361845E-17));
#7091=CARTESIAN_POINT('Ctrl Pts',(2.34404815214704,-1.09970570501749,-1.73347562424884E-16));
#7092=CARTESIAN_POINT('Ctrl Pts',(2.38703114656335,-1.02177339518613,-6.93889390390723E-17));
#7093=CARTESIAN_POINT('Ctrl Pts',(2.40590762936263,-0.98754851332257,-2.37342983415729E-17));
#7094=CARTESIAN_POINT('Ctrl Pts',(2.42404566668818,-0.95287338422101,-3.73213098570097E-17));
#7095=CARTESIAN_POINT('Ctrl Pts',(2.44143777842235,-0.917776011982524,-2.77555756156289E-17));
#7096=CARTESIAN_POINT('Ctrl Pts',(2.45136231257179,-0.897748250278805,-2.22970402983493E-17));
#7097=CARTESIAN_POINT('Ctrl Pts',(2.46104392774577,-0.87758297572818,-3.33298356902162E-16));
#7098=CARTESIAN_POINT('Ctrl Pts',(2.47048100099708,-0.857285244332943,-3.46944695195361E-16));
#7099=CARTESIAN_POINT('Ctrl Pts',(2.47900168762219,-0.838958523344988,-3.59265906346346E-16));
#7100=CARTESIAN_POINT('Ctrl Pts',(2.48732540306445,-0.820518075787568,-6.44662433235081E-16));
#7101=CARTESIAN_POINT('Ctrl Pts',(2.49543725255318,-0.801999440640286,-6.24500451351651E-16));
#7102=CARTESIAN_POINT('Ctrl Pts',(2.53203160380214,-0.71845777234719,-5.33545281640661E-16));
#7103=CARTESIAN_POINT('Ctrl Pts',(2.56436439720616,-0.633232805885642,-1.7353518107917E-16));
#7104=CARTESIAN_POINT('Ctrl Pts',(2.59240963609592,-0.546722656501286,-2.22044604925031E-16));
#7105=CARTESIAN_POINT('Ctrl Pts',(2.62091418406923,-0.458795692748289,-2.71348488718176E-16));
#7106=CARTESIAN_POINT('Ctrl Pts',(2.64499008370221,-0.369540350457117,-6.24020080701783E-16));
#7107=CARTESIAN_POINT('Ctrl Pts',(2.66457097387791,-0.279337521515105,-6.66133814775094E-16));
#7108=CARTESIAN_POINT('Ctrl Pts',(2.68356661536034,-0.191830744044346,-7.06988821200503E-16));
#7109=CARTESIAN_POINT('Ctrl Pts',(2.69833209310255,-0.103431355980504,-8.41126525273291E-16));
#7110=CARTESIAN_POINT('Ctrl Pts',(2.70876601617631,-0.0144652215165946,
-9.29811783123569E-16));
#7111=CARTESIAN_POINT('Ctrl Pts',(2.71312946546923,0.0227402680942152,-9.66899810601249E-16));
#7112=CARTESIAN_POINT('Ctrl Pts',(2.71673485533152,0.0600450673053063,-4.75178540744584E-16));
#7113=CARTESIAN_POINT('Ctrl Pts',(2.71957245241254,0.0974259566605276,-4.71844785465692E-16));
#7114=CARTESIAN_POINT('Ctrl Pts',(2.72134694520476,0.120802115020483,-4.69760019889566E-16));
#7115=CARTESIAN_POINT('Ctrl Pts',(2.7228211544872,0.144208034837555,-4.55034229124723E-16));
#7116=CARTESIAN_POINT('Ctrl Pts',(2.7239924097264,0.167638070156344,-4.44089209850063E-16));
#7117=CARTESIAN_POINT('Ctrl Pts',(2.72467909724156,0.181374711150338,-4.37672326631462E-16));
#7118=CARTESIAN_POINT('Ctrl Pts',(2.72526137600902,0.195115066492318,-8.40764763959006E-16));
#7119=CARTESIAN_POINT('Ctrl Pts',(2.72573871993999,0.208849770915952,-8.32667268468867E-16));
#7120=CARTESIAN_POINT('Ctrl Pts',(2.72911188874676,0.305906575299357,-7.75446012623746E-16));
#7121=CARTESIAN_POINT('Ctrl Pts',(2.7272553636767,0.402801526105327,-9.68836665814074E-16));
#7122=CARTESIAN_POINT('Ctrl Pts',(2.72010339077746,0.499113381476287,-9.15933995315754E-16));
#7123=CARTESIAN_POINT('Ctrl Pts',(2.71295141787821,0.595425236847248,-8.63031324817435E-16));
#7124=CARTESIAN_POINT('Ctrl Pts',(2.70050443398604,0.691155049107752,-7.97669397634917E-16));
#7125=CARTESIAN_POINT('Ctrl Pts',(2.68264379028147,0.785900518836936,-7.7715611723761E-16));
#7126=CARTESIAN_POINT('Ctrl Pts',(2.66557036541062,0.876470023835268,-7.30823456910502E-16));
#7127=CARTESIAN_POINT('Ctrl Pts',(2.64355009898795,0.966141014464811,-6.44790703633136E-16));
#7128=CARTESIAN_POINT('Ctrl Pts',(2.61685826648582,1.0546735630477,-5.82867087928207E-16));
#7129=CARTESIAN_POINT('Ctrl Pts',(2.60792689184721,1.08429750734011,-5.62146779167304E-16));
#7130=CARTESIAN_POINT('Ctrl Pts',(2.59847203287526,1.11379395063906,-3.30994876511457E-16));
#7131=CARTESIAN_POINT('Ctrl Pts',(2.58850272866474,1.14315372665541,-3.33066907387547E-16));
#7132=CARTESIAN_POINT('Ctrl Pts',(2.58205412116549,1.16214498901409,-3.34407192884316E-16));
#7133=CARTESIAN_POINT('Ctrl Pts',(2.57539025197676,1.18107906596373,-3.83440297547856E-16));
#7134=CARTESIAN_POINT('Ctrl Pts',(2.56851343345694,1.1999534423939,-3.88578058618805E-16));
#7135=CARTESIAN_POINT('Ctrl Pts',(2.56187577896064,1.21817140019159,-3.93537137119301E-16));
#7136=CARTESIAN_POINT('Ctrl Pts',(2.5550379237584,1.23633808433789,-5.11405226480168E-17));
#7137=CARTESIAN_POINT('Ctrl Pts',(2.54801290532315,1.2544236637051,-8.32667268468867E-17));
#7138=CARTESIAN_POINT('Ctrl Pts',(2.51416596007442,1.34156103142528,-2.38052637316906E-16));
#7139=CARTESIAN_POINT('Ctrl Pts',(2.47593990461506,1.42692801454723,-3.20308050061359E-16));
#7140=CARTESIAN_POINT('Ctrl Pts',(2.43366643270999,1.51029042462874,-3.60822483003176E-16));
#7141=CARTESIAN_POINT('Ctrl Pts',(2.38981735466084,1.59675989735712,-4.02846959634101E-16));
#7142=CARTESIAN_POINT('Ctrl Pts',(2.34161340681444,1.68107330940561,-3.78619360334886E-16));
#7143=CARTESIAN_POINT('Ctrl Pts',(2.28936877468746,1.76296634463835,-4.16333634234434E-16));
#7144=CARTESIAN_POINT('Ctrl Pts',(2.23653118032041,1.84578884335166,-4.54475954794925E-16));
#7145=CARTESIAN_POINT('Ctrl Pts',(2.17956025026491,1.92613653330701,-4.81277067279742E-16));
#7146=CARTESIAN_POINT('Ctrl Pts',(2.11872917895946,2.00372118802566,-3.33066907387547E-16));
#7147=CARTESIAN_POINT('Ctrl Pts',(2.07707986191238,2.05684121062297,-2.31591595405106E-16));
#7148=CARTESIAN_POINT('Ctrl Pts',(2.03361992333023,2.10866568467281,-4.99150862322262E-16));
#7149=CARTESIAN_POINT('Ctrl Pts',(1.98842485791504,2.15909508034387,-5.55111512312578E-16));
#7150=CARTESIAN_POINT('Ctrl Pts',(1.97697062272433,2.17187590394121,-5.69294176736786E-16));
#7151=CARTESIAN_POINT('Ctrl Pts',(1.96540341059899,2.18456858588751,-5.43387176388567E-16));
#7152=CARTESIAN_POINT('Ctrl Pts',(1.95373682360776,2.19715826975418,-5.55111512312578E-16));
#7153=CARTESIAN_POINT('Ctrl Pts',(1.88513632513593,2.27118665436278,-6.24051579295601E-16));
#7154=CARTESIAN_POINT('Ctrl Pts',(1.81301954111561,2.34175145938146,-9.96121943412486E-16));
#7155=CARTESIAN_POINT('Ctrl Pts',(1.7376981084074,2.40856242043656,-8.32667268468867E-16));
#7156=CARTESIAN_POINT('Ctrl Pts',(1.67462785275174,2.4645064491524,-6.95798813287656E-16));
#7157=CARTESIAN_POINT('Ctrl Pts',(1.60930957241425,2.51781846345041,-7.13394759801054E-17));
#7158=CARTESIAN_POINT('Ctrl Pts',(1.54190225473945,2.56831419612331,-5.55111512312578E-17));
#7159=CARTESIAN_POINT('Ctrl Pts',(1.50803147786761,2.59368725283794,-4.75577468485228E-17));
#7160=CARTESIAN_POINT('Ctrl Pts',(1.47363293052346,2.61834900472236,-3.20435029838497E-16));
#7161=CARTESIAN_POINT('Ctrl Pts',(1.43872500006545,2.64227442481775,-3.33066907387547E-16));
#7162=CARTESIAN_POINT('Ctrl Pts',(1.42333727249881,2.6528209637135,-3.38635151847466E-16));
#7163=CARTESIAN_POINT('Ctrl Pts',(1.40785826547886,2.66321910753516,-4.40548340244713E-16));
#7164=CARTESIAN_POINT('Ctrl Pts',(1.3922911852266,2.67346618319487,-3.88578058618805E-16));
#7165=CARTESIAN_POINT('Ctrl Pts',(1.30709626507894,2.72954598611418,-1.04157093259739E-16));
#7166=CARTESIAN_POINT('Ctrl Pts',(1.21925397020065,2.78111238575669,5.889711510458E-17));
#7167=CARTESIAN_POINT('Ctrl Pts',(1.12905315937313,2.8278552735782,5.55111512312578E-17));
#7168=CARTESIAN_POINT('Ctrl Pts',(1.04989346616971,2.86887655293752,5.25396495457291E-17));
#7169=CARTESIAN_POINT('Ctrl Pts',(0.968916412162158,2.90618287529182,-1.56714687611455E-16));
#7170=CARTESIAN_POINT('Ctrl Pts',(0.886294660306285,2.939540402264,-2.77555756156289E-16));
#7171=CARTESIAN_POINT('Ctrl Pts',(0.856267218376713,2.95166361656982,-3.21473345494835E-16));
#7172=CARTESIAN_POINT('Ctrl Pts',(0.826022362315256,2.96326500943248,-4.61516649787808E-17));
#7173=CARTESIAN_POINT('Ctrl Pts',(0.795572458610595,2.9743481795293,-5.55111512312578E-17));
#7174=CARTESIAN_POINT('Ctrl Pts',(-2.51342302570288,-0.000307789261743824,
8.61258330249198));
#7175=CARTESIAN_POINT('Ctrl Pts',(-2.51312706795389,0.431039503037857,8.58541917613674));
#7176=CARTESIAN_POINT('Ctrl Pts',(-2.40775786821181,0.862561153211593,8.5582550497815));
#7177=CARTESIAN_POINT('Ctrl Pts',(-2.19819431079963,1.23549101176992,8.53109092342626));
#7178=CARTESIAN_POINT('Ctrl Pts',(-1.79192915447086,1.95846216743165,8.47842986834338));
#7179=CARTESIAN_POINT('Ctrl Pts',(-0.994073784189135,2.46122972735536,8.42576881326051));
#7180=CARTESIAN_POINT('Ctrl Pts',(-0.166600750120509,2.51599743782446,8.37310775817763));
#7181=CARTESIAN_POINT('Ctrl Pts',(0.660872283948123,2.57076514829355,8.32044670309475));
#7182=CARTESIAN_POINT('Ctrl Pts',(1.51796298180366,2.17753300930801,8.26778564801187));
#7183=CARTESIAN_POINT('Ctrl Pts',(2.01603480884577,1.51452492004508,8.21512459292899));
#7184=CARTESIAN_POINT('Ctrl Pts',(2.51410663588786,0.85151683078216,8.16246353784611));
#7185=CARTESIAN_POINT('Ctrl Pts',(2.65315959211654,-0.0812672087581283,
8.10980248276323));
#7186=CARTESIAN_POINT('Ctrl Pts',(2.37009487307924,-0.860734358319284,8.05714142768036));
#7187=CARTESIAN_POINT('Ctrl Pts',(2.08703015404192,-1.64020150788046,8.00448037259748));
#7188=CARTESIAN_POINT('Ctrl Pts',(1.38184775973859,-2.26635176746249,7.9518193175146));
#7189=CARTESIAN_POINT('Ctrl Pts',(0.574378711156563,-2.4552463309339,7.89915826243172));
#7190=CARTESIAN_POINT('Ctrl Pts',(-0.233090337425462,-2.64414089440531,
7.84649720734884));
#7191=CARTESIAN_POINT('Ctrl Pts',(-1.1428460402862,-2.39577976176609,7.79383615226596));
#7192=CARTESIAN_POINT('Ctrl Pts',(-1.7423084702292,-1.82278273195717,7.74117509718308));
#7193=CARTESIAN_POINT('Ctrl Pts',(-2.23024621723499,-1.35638673147292,7.69831116561938));
#7194=CARTESIAN_POINT('Ctrl Pts',(-2.51260567208493,-0.674910034313931,
7.65544723405568));
#7195=CARTESIAN_POINT('Ctrl Pts',(-2.5186623288877,0.00210982157644382,
7.61258330249198));
#7196=CARTESIAN_POINT('Ctrl Pts',(-0.793799282532843,2.9692229537457,-1.11022302462516E-15));
#7197=CARTESIAN_POINT('Ctrl Pts',(-1.77625330176029,2.70657130793364,0.0526610550828771));
#7198=CARTESIAN_POINT('Ctrl Pts',(-3.44352486880409,1.13462630258776,0.157983165248634));
#7199=CARTESIAN_POINT('Ctrl Pts',(-2.83104022223192,-2.27044164625735,0.315966330497268));
#7200=CARTESIAN_POINT('Ctrl Pts',(0.353891905593742,-3.60835904048448,0.473949495745902));
#7201=CARTESIAN_POINT('Ctrl Pts',(3.21549712367075,-1.67724424006994,0.631932660994537));
#7202=CARTESIAN_POINT('Ctrl Pts',(3.16174910309101,1.77718997587638,0.789915826243172));
#7203=CARTESIAN_POINT('Ctrl Pts',(0.239554143273228,3.61860888141612,0.947898991491804));
#7204=CARTESIAN_POINT('Ctrl Pts',(-2.8995942030829,2.17837084084757,1.10588215674044));
#7205=CARTESIAN_POINT('Ctrl Pts',(-3.40888424173261,-1.23800851265563,1.26386532198907));
#7206=CARTESIAN_POINT('Ctrl Pts',(-0.82610974606013,-3.53132320122762,1.42184848723771));
#7207=CARTESIAN_POINT('Ctrl Pts',(2.50592737524966,-2.62168489533313,1.57983165248634));
#7208=CARTESIAN_POINT('Ctrl Pts',(3.56502744730094,0.665951678041991,1.73781481773498));
#7209=CARTESIAN_POINT('Ctrl Pts',(1.3905130838547,3.34952614641417,1.89579798298361));
#7210=CARTESIAN_POINT('Ctrl Pts',(-2.04523738986722,2.99497715066286,2.05378114823225));
#7211=CARTESIAN_POINT('Ctrl Pts',(-3.62589125240128,-0.0761241329263979,
2.21176431348088));
#7212=CARTESIAN_POINT('Ctrl Pts',(-1.9177361559176,-3.07817520619115,2.36974747872952));
#7213=CARTESIAN_POINT('Ctrl Pts',(1.52987013245233,-3.28821788231848,2.52773064397815));
#7214=CARTESIAN_POINT('Ctrl Pts',(3.58983249342927,-0.515733880008737,2.68571380922678));
#7215=CARTESIAN_POINT('Ctrl Pts',(2.39369399271082,2.72453792342614,2.84369697447542));
#7216=CARTESIAN_POINT('Ctrl Pts',(-0.973606524696896,3.49356106124283,3.00168013972405));
#7217=CARTESIAN_POINT('Ctrl Pts',(-3.45781276429597,1.09380495610431,3.15966330497269));
#7218=CARTESIAN_POINT('Ctrl Pts',(-2.80566476683024,-2.29806951664741,3.31764647022132));
#7219=CARTESIAN_POINT('Ctrl Pts',(0.39131691802336,-3.60551653188198,3.47562963546996));
#7220=CARTESIAN_POINT('Ctrl Pts',(3.23336081192176,-1.64263697190919,3.63361280071859));
#7221=CARTESIAN_POINT('Ctrl Pts',(3.14263608255428,1.81017037953698,3.79159596596722));
#7222=CARTESIAN_POINT('Ctrl Pts',(0.20143316418192,3.62109141633224,3.94957913121586));
#7223=CARTESIAN_POINT('Ctrl Pts',(-2.92247651090087,2.14755894050069,4.1075622964645));
#7224=CARTESIAN_POINT('Ctrl Pts',(-3.39560023944938,-1.27388279388956,4.26554546171314));
#7225=CARTESIAN_POINT('Ctrl Pts',(-0.788798652099944,-3.53986935455429,
4.42352862696176));
#7226=CARTESIAN_POINT('Ctrl Pts',(2.53347023630324,-2.59507358691089,4.5815117922104));
#7227=CARTESIAN_POINT('Ctrl Pts',(3.55779514749501,0.703542499198116,4.73949495745903));
#7228=CARTESIAN_POINT('Ctrl Pts',(1.35507842480211,3.36402152542208,4.89747812270768));
#7229=CARTESIAN_POINT('Ctrl Pts',(-2.07674068097001,2.97321820637517,5.05546128795629));
#7230=CARTESIAN_POINT('Ctrl Pts',(-3.62488510543213,-0.114395507376902,
5.21344445320494));
#7231=CARTESIAN_POINT('Ctrl Pts',(-1.88513501425953,-3.09824859284726,5.37142761845357));
#7232=CARTESIAN_POINT('Ctrl Pts',(1.56449687870927,-3.27188445193808,5.52941078370221));
#7233=CARTESIAN_POINT('Ctrl Pts',(3.59507670274909,-0.477809442042676,5.68739394895084));
#7234=CARTESIAN_POINT('Ctrl Pts',(2.36479925030647,2.74965505068462,5.84537711419948));
#7235=CARTESIAN_POINT('Ctrl Pts',(-1.01043183895086,3.48308854122473,6.00336027944811));
#7236=CARTESIAN_POINT('Ctrl Pts',(-3.469166759934,1.05724187710076,6.16134344469674));
#7237=CARTESIAN_POINT('Ctrl Pts',(-2.78124902365658,-2.32755932727262,6.31932660994538));
#7238=CARTESIAN_POINT('Ctrl Pts',(0.429356514911867,-3.60118463981366,6.47730977519402));
#7239=CARTESIAN_POINT('Ctrl Pts',(3.25052102458439,-1.60841283090018,6.63529294044265));
#7240=CARTESIAN_POINT('Ctrl Pts',(3.12335204644367,1.8432448176368,6.79327610569127));
#7241=CARTESIAN_POINT('Ctrl Pts',(0.163196100475927,3.6230155390935,6.95125927093992));
#7242=CARTESIAN_POINT('Ctrl Pts',(-2.944984173578,2.11658934969185,7.10924243618855));
#7243=CARTESIAN_POINT('Ctrl Pts',(-3.38196348508519,-1.30965915392286,7.26722560143719));
#7244=CARTESIAN_POINT('Ctrl Pts',(-0.751386096246847,-3.5479953461427,7.42520876668581));
#7245=CARTESIAN_POINT('Ctrl Pts',(2.56072339002455,-2.56819159278999,7.58319193193446));
#7246=CARTESIAN_POINT('Ctrl Pts',(3.55017077169744,0.741074350000556,7.74117509718308));
#7247=CARTESIAN_POINT('Ctrl Pts',(1.31948938364505,3.37811317609581,7.89915826243173));
#7248=CARTESIAN_POINT('Ctrl Pts',(-2.10800873502834,2.95117875161517,8.05714142768035));
#7249=CARTESIAN_POINT('Ctrl Pts',(-3.62348089025001,-0.152749143368613,
8.21512459292899));
#7250=CARTESIAN_POINT('Ctrl Pts',(-1.85231323033622,-3.11779603581512,8.37310775817763));
#7251=CARTESIAN_POINT('Ctrl Pts',(1.59892942568934,-3.25553164520284,8.53109092342626));
#7252=CARTESIAN_POINT('Ctrl Pts',(3.59995819558759,-0.439170790472673,8.68907408867489));
#7253=CARTESIAN_POINT('Ctrl Pts',(2.33556733953737,2.77319664798175,8.84705725392354));
#7254=CARTESIAN_POINT('Ctrl Pts',(-1.04699337368903,3.47469407062061,9.00504041917216));
#7255=CARTESIAN_POINT('Ctrl Pts',(-3.48051498243553,1.01550766892132,9.1630235844208));
#7256=CARTESIAN_POINT('Ctrl Pts',(-2.99692813421427,-1.22434708939046,9.26834569458656));
#7257=CARTESIAN_POINT('Ctrl Pts',(-2.33606265769612,-1.99730155693068,9.32100674966943));
#7258=CARTESIAN_POINT('Ctrl Pts',(-0.745932854346924,2.79017756984216,-0.107002249889812));
#7259=CARTESIAN_POINT('Ctrl Pts',(-1.66914448599339,2.5433639279422,-0.0543411948069335));
#7260=CARTESIAN_POINT('Ctrl Pts',(-3.23587888137879,1.06620786278094,0.0509809153588226));
#7261=CARTESIAN_POINT('Ctrl Pts',(-2.66032731473656,-2.13353306696999,0.208964080607457));
#7262=CARTESIAN_POINT('Ctrl Pts',(0.33255207591963,-3.39077348368069,0.366947245856092));
#7263=CARTESIAN_POINT('Ctrl Pts',(3.02160130448948,-1.57610571206399,0.524930411104726));
#7264=CARTESIAN_POINT('Ctrl Pts',(2.97109431199307,1.67002467826918,0.682913576353362));
#7265=CARTESIAN_POINT('Ctrl Pts',(0.225108928408532,3.40040525492435,0.840896741601994));
#7266=CARTESIAN_POINT('Ctrl Pts',(-2.72474746191766,2.04701416957039,0.998879906850632));
#7267=CARTESIAN_POINT('Ctrl Pts',(-3.20332709858383,-1.1633560824147,1.15686307209926));
#7268=CARTESIAN_POINT('Ctrl Pts',(-0.776294983432353,-3.31838293769717,
1.3148462373479));
#7269=CARTESIAN_POINT('Ctrl Pts',(2.3548189081775,-2.46359620146564,1.47282940259653));
#7270=CARTESIAN_POINT('Ctrl Pts',(3.35005480365913,0.625794513789364,1.63081256784517));
#7271=CARTESIAN_POINT('Ctrl Pts',(1.30666456429251,3.14754832119794,1.7887957330938));
#7272=CARTESIAN_POINT('Ctrl Pts',(-1.92190872127375,2.8143787779316,1.94677889834244));
#7273=CARTESIAN_POINT('Ctrl Pts',(-3.40724849589837,-0.0715338159254679,
2.10476206359107));
#7274=CARTESIAN_POINT('Ctrl Pts',(-1.80209586496915,-2.89255995597237,2.26274522883971));
#7275=CARTESIAN_POINT('Ctrl Pts',(1.43761832467147,-3.08993697102635,2.42072839408834));
#7276=CARTESIAN_POINT('Ctrl Pts',(3.37336409514862,-0.484634911700634,2.57871155933697));
#7277=CARTESIAN_POINT('Ctrl Pts',(2.24935324546856,2.56024714901858,2.73669472458561));
#7278=CARTESIAN_POINT('Ctrl Pts',(-0.914897644730358,3.28289787052096,2.89467788983424));
#7279=CARTESIAN_POINT('Ctrl Pts',(-3.24930521080662,1.02784806053531,3.05266105508288));
#7280=CARTESIAN_POINT('Ctrl Pts',(-2.63648200989107,-2.15949496523957,3.21064422033151));
#7281=CARTESIAN_POINT('Ctrl Pts',(0.367720344473012,-3.3881023795338,3.36862738558015));
#7282=CARTESIAN_POINT('Ctrl Pts',(3.03838780488001,-1.54358527662352,3.52661055082878));
#7283=CARTESIAN_POINT('Ctrl Pts',(2.95313381457531,1.70101634981814,3.68459371607742));
#7284=CARTESIAN_POINT('Ctrl Pts',(0.189286660273763,3.40273809194845,3.84257688132605));
#7285=CARTESIAN_POINT('Ctrl Pts',(-2.74624995701975,2.01806023967986,4.00056004657468));
#7286=CARTESIAN_POINT('Ctrl Pts',(-3.19084412718499,-1.19706712951099,4.15854321182332));
#7287=CARTESIAN_POINT('Ctrl Pts',(-0.74123376401713,-3.32641375440981,4.31652637707195));
#7288=CARTESIAN_POINT('Ctrl Pts',(2.38070092320909,-2.43858956605276,4.47450954232059));
#7289=CARTESIAN_POINT('Ctrl Pts',(3.34325861455133,0.661118592733809,4.63249270756923));
#7290=CARTESIAN_POINT('Ctrl Pts',(1.27336662997645,3.16116962279916,4.79047587281786));
#7291=CARTESIAN_POINT('Ctrl Pts',(-1.9515123507689,2.79393190706986,4.94845903806649));
#7292=CARTESIAN_POINT('Ctrl Pts',(-3.40630302001157,-0.107497410516475,
5.10644220331512));
#7293=CARTESIAN_POINT('Ctrl Pts',(-1.7714605857656,-2.91142290903152,5.26442536856377));
#7294=CARTESIAN_POINT('Ctrl Pts',(1.47015706367078,-3.07458845331788,5.42240853381239));
#7295=CARTESIAN_POINT('Ctrl Pts',(3.37829207645675,-0.448997333179196,5.58039169906104));
#7296=CARTESIAN_POINT('Ctrl Pts',(2.22220086809614,2.58384970301577,5.73837486430966));
#7297=CARTESIAN_POINT('Ctrl Pts',(-0.949502377158481,3.27305684783272,5.89635802955831));
#7298=CARTESIAN_POINT('Ctrl Pts',(-3.25997455576684,0.993489750462507,6.05434119480693));
#7299=CARTESIAN_POINT('Ctrl Pts',(-2.61353854622553,-2.18720652797068,6.21232436005557));
#7300=CARTESIAN_POINT('Ctrl Pts',(0.403466137785788,-3.38403170236597,6.3703075253042));
#7301=CARTESIAN_POINT('Ctrl Pts',(3.05451324955387,-1.51142486560757,6.52829069055284));
#7302=CARTESIAN_POINT('Ctrl Pts',(2.93501261389417,1.73209638549038,6.68627385580147));
#7303=CARTESIAN_POINT('Ctrl Pts',(0.153355307475048,3.40454618930379,6.84425702105011));
#7304=CARTESIAN_POINT('Ctrl Pts',(-2.76740039823942,1.98895812812809,7.00224018629874));
#7305=CARTESIAN_POINT('Ctrl Pts',(-3.17802967480296,-1.23068616009594,7.16022335154738));
#7306=CARTESIAN_POINT('Ctrl Pts',(-0.706077200903509,-3.33404974531244,
7.318206516796));
#7307=CARTESIAN_POINT('Ctrl Pts',(2.40631070038151,-2.41332856740186,7.47618968204465));
#7308=CARTESIAN_POINT('Ctrl Pts',(3.33609399179789,0.696387257261517,7.63417284729327));
#7309=CARTESIAN_POINT('Ctrl Pts',(1.23992362286129,3.17441154105332,7.79215601254192));
#7310=CARTESIAN_POINT('Ctrl Pts',(-1.98089492811161,2.77322144063441,7.95013917779054));
#7311=CARTESIAN_POINT('Ctrl Pts',(-3.40498347959126,-0.143538306243407,
8.10812234303918));
#7312=CARTESIAN_POINT('Ctrl Pts',(-1.74061796911753,-2.92979163302642,8.26610550828781));
#7313=CARTESIAN_POINT('Ctrl Pts',(1.50251331369072,-3.05922172765686,8.42408867353645));
#7314=CARTESIAN_POINT('Ctrl Pts',(3.38287921323883,-0.412688608432349,8.58207183878508));
#7315=CARTESIAN_POINT('Ctrl Pts',(2.19473165375214,2.60597173216614,8.74005500403373));
#7316=CARTESIAN_POINT('Ctrl Pts',(-0.983859236085748,3.26516856731113,8.89803816928235));
#7317=CARTESIAN_POINT('Ctrl Pts',(-3.2706384757131,0.954272132462314,9.05602133453099));
#7318=CARTESIAN_POINT('Ctrl Pts',(-2.81621211636024,-1.15051844867672,9.16134344469675));
#7319=CARTESIAN_POINT('Ctrl Pts',(-2.1951971040191,-1.87686343907878,9.21400449977962));
#7320=CARTESIAN_POINT('Ctrl Pts',(-0.698066426161006,2.61113218593862,-0.214004499779622));
#7321=CARTESIAN_POINT('Ctrl Pts',(-1.56203567022649,2.38015654795075,-0.161343444696744));
#7322=CARTESIAN_POINT('Ctrl Pts',(-3.02823289395347,0.997789422974118,-0.0560213345309879));
#7323=CARTESIAN_POINT('Ctrl Pts',(-2.48961440724121,-1.99662448768263,0.101961830717646));
#7324=CARTESIAN_POINT('Ctrl Pts',(0.311212246245525,-3.1731879268769,0.259944995966281));
#7325=CARTESIAN_POINT('Ctrl Pts',(2.8277054853082,-1.47496718405804,0.417928161214915));
#7326=CARTESIAN_POINT('Ctrl Pts',(2.78043952089512,1.56285938066197,0.57591132646355));
#7327=CARTESIAN_POINT('Ctrl Pts',(0.210663713543839,3.18220162843258,0.733894491712185));
#7328=CARTESIAN_POINT('Ctrl Pts',(-2.54990072075242,1.91565749829321,0.891877656960819));
#7329=CARTESIAN_POINT('Ctrl Pts',(-2.99776995543505,-1.08870365217376,1.04986082220945));
#7330=CARTESIAN_POINT('Ctrl Pts',(-0.726480220804574,-3.10544267416671,
1.20784398745809));
#7331=CARTESIAN_POINT('Ctrl Pts',(2.20371044110535,-2.30550750759815,1.36582715270672));
#7332=CARTESIAN_POINT('Ctrl Pts',(3.13508216001732,0.585637349536739,1.52381031795536));
#7333=CARTESIAN_POINT('Ctrl Pts',(1.22281604473031,2.9455704959817,1.68179348320399));
#7334=CARTESIAN_POINT('Ctrl Pts',(-1.79858005268027,2.63378040520035,1.83977664845263));
#7335=CARTESIAN_POINT('Ctrl Pts',(-3.18860573939546,-0.0669434989245405,
1.99775981370126));
#7336=CARTESIAN_POINT('Ctrl Pts',(-1.6864555740207,-2.70694470575358,2.1557429789499));
#7337=CARTESIAN_POINT('Ctrl Pts',(1.3453665168906,-2.89165605973422,2.31372614419853));
#7338=CARTESIAN_POINT('Ctrl Pts',(3.15689569686798,-0.453535943392533,2.47170930944716));
#7339=CARTESIAN_POINT('Ctrl Pts',(2.10501249822631,2.39595637461102,2.6296924746958));
#7340=CARTESIAN_POINT('Ctrl Pts',(-0.856188764763818,3.07223467979908,2.78767563994443));
#7341=CARTESIAN_POINT('Ctrl Pts',(-3.04079765731727,0.961891164966307,2.94565880519307));
#7342=CARTESIAN_POINT('Ctrl Pts',(-2.4672992529519,-2.02092041383173,3.1036419704417));
#7343=CARTESIAN_POINT('Ctrl Pts',(0.344123770922663,-3.17068822718562,3.26162513569034));
#7344=CARTESIAN_POINT('Ctrl Pts',(2.84341479783825,-1.44453358133785,3.41960830093897));
#7345=CARTESIAN_POINT('Ctrl Pts',(2.76363154659633,1.5918623200993,3.5775914661876));
#7346=CARTESIAN_POINT('Ctrl Pts',(0.177140156365606,3.18438476756466,3.73557463143624));
#7347=CARTESIAN_POINT('Ctrl Pts',(-2.57002340313862,1.88856153885904,3.89355779668487));
#7348=CARTESIAN_POINT('Ctrl Pts',(-2.9860880149206,-1.12025146513243,4.05154096193351));
#7349=CARTESIAN_POINT('Ctrl Pts',(-0.693668875934318,-3.11295815426533,
4.20952412718214));
#7350=CARTESIAN_POINT('Ctrl Pts',(2.22793161011494,-2.28210554519462,4.36750729243078));
#7351=CARTESIAN_POINT('Ctrl Pts',(3.12872208160764,0.6186946862695,4.52549045767941));
#7352=CARTESIAN_POINT('Ctrl Pts',(1.1916548351508,2.95831772017624,4.68347362292805));
#7353=CARTESIAN_POINT('Ctrl Pts',(-1.8262840205678,2.61464560776455,4.84145678817668));
#7354=CARTESIAN_POINT('Ctrl Pts',(-3.18772093459101,-0.100599313656048,
4.99943995342532));
#7355=CARTESIAN_POINT('Ctrl Pts',(-1.65778615727167,-2.72459722521578,5.15742311867394));
#7356=CARTESIAN_POINT('Ctrl Pts',(1.3758172486323,-2.87729245469768,5.31540628392259));
#7357=CARTESIAN_POINT('Ctrl Pts',(3.16150745016441,-0.420185224315714,5.47338944917121));
#7358=CARTESIAN_POINT('Ctrl Pts',(2.0796024858858,2.41804435534692,5.63137261441986));
#7359=CARTESIAN_POINT('Ctrl Pts',(-0.888572915366094,3.06302515444072,5.78935577966849));
#7360=CARTESIAN_POINT('Ctrl Pts',(-3.05078235159968,0.929737623824253,5.94733894491712));
#7361=CARTESIAN_POINT('Ctrl Pts',(-2.44582806879447,-2.04685372866874,6.10532211016575));
#7362=CARTESIAN_POINT('Ctrl Pts',(0.377575760659711,-3.16687876491828,6.2633052754144));
#7363=CARTESIAN_POINT('Ctrl Pts',(2.85850547452334,-1.41443690031496,6.42128844066302));
#7364=CARTESIAN_POINT('Ctrl Pts',(2.74667318134467,1.62094795334397,6.57927160591167));
#7365=CARTESIAN_POINT('Ctrl Pts',(0.143514514474167,3.18607683951409,6.73725477116029));
#7366=CARTESIAN_POINT('Ctrl Pts',(-2.58981662290085,1.86132690656433,6.89523793640893));
#7367=CARTESIAN_POINT('Ctrl Pts',(-2.97409586452072,-1.15171316626902,7.05322110165757));
#7368=CARTESIAN_POINT('Ctrl Pts',(-0.660768305560169,-3.12010414448219,
7.2112042669062));
#7369=CARTESIAN_POINT('Ctrl Pts',(2.25189801073846,-2.25846554201373,7.36918743215484));
#7370=CARTESIAN_POINT('Ctrl Pts',(3.12201721189835,0.65170016452248,7.52717059740346));
#7371=CARTESIAN_POINT('Ctrl Pts',(1.16035786207753,2.97070990601083,7.68515376265211));
#7372=CARTESIAN_POINT('Ctrl Pts',(-1.85378112119487,2.59526412965366,7.84313692790074));
#7373=CARTESIAN_POINT('Ctrl Pts',(-3.18648606893251,-0.134327469118203,
8.00112009314937));
#7374=CARTESIAN_POINT('Ctrl Pts',(-1.62892270789884,-2.74178723023772,8.159103258398));
#7375=CARTESIAN_POINT('Ctrl Pts',(1.4060972016921,-2.86291181011087,8.31708642364665));
#7376=CARTESIAN_POINT('Ctrl Pts',(3.16580023089008,-0.386206426392027,8.47506958889527));
#7377=CARTESIAN_POINT('Ctrl Pts',(2.0538959679669,2.43874681635053,8.63305275414391));
#7378=CARTESIAN_POINT('Ctrl Pts',(-0.92072509848246,3.05564306400165,8.79103591939254));
#7379=CARTESIAN_POINT('Ctrl Pts',(-3.06076196899067,0.893036596003309,8.94901908464118));
#7380=CARTESIAN_POINT('Ctrl Pts',(-2.6354960985062,-1.07668980796297,9.05434119480693));
#7381=CARTESIAN_POINT('Ctrl Pts',(-2.05433155034207,-1.75642532122688,9.10700224988981));
#7382=CARTESIAN_POINT('Ctrl Pts',(-0.650199997975088,2.43208680203507,-0.321006749669433));
#7383=CARTESIAN_POINT('Ctrl Pts',(-1.45492685445959,2.21694916795931,-0.268345694586555));
#7384=CARTESIAN_POINT('Ctrl Pts',(-2.82058690652816,0.929370983167296,-0.163023584420799));
#7385=CARTESIAN_POINT('Ctrl Pts',(-2.31890149974585,-1.85971590839527,-0.00504041917216426));
#7386=CARTESIAN_POINT('Ctrl Pts',(0.289872416571416,-2.9556023700731,0.15294274607647));
#7387=CARTESIAN_POINT('Ctrl Pts',(2.63380966612693,-1.37382865605209,0.310925911325105));
#7388=CARTESIAN_POINT('Ctrl Pts',(2.58978472979718,1.45569408305476,0.468909076573739));
#7389=CARTESIAN_POINT('Ctrl Pts',(0.196218498679142,2.96399800194081,0.626892241822374));
#7390=CARTESIAN_POINT('Ctrl Pts',(-2.37505397958718,1.78430082701602,0.784875407071009));
#7391=CARTESIAN_POINT('Ctrl Pts',(-2.79221281228627,-1.01405122193283,0.942858572319641));
#7392=CARTESIAN_POINT('Ctrl Pts',(-0.676665458176792,-2.89250241063626,
1.10084173756828));
#7393=CARTESIAN_POINT('Ctrl Pts',(2.05260197403319,-2.14741881373065,1.25882490281691));
#7394=CARTESIAN_POINT('Ctrl Pts',(2.92010951637551,0.545480185284112,1.41680806806555));
#7395=CARTESIAN_POINT('Ctrl Pts',(1.13896752516812,2.74359267076547,1.57479123331418));
#7396=CARTESIAN_POINT('Ctrl Pts',(-1.67525138408679,2.45318203246909,1.73277439856282));
#7397=CARTESIAN_POINT('Ctrl Pts',(-2.96996298289254,-0.0623531819236091,
1.89075756381145));
#7398=CARTESIAN_POINT('Ctrl Pts',(-1.57081528307225,-2.5213294555348,2.04874072906008));
#7399=CARTESIAN_POINT('Ctrl Pts',(1.25311470910973,-2.6933751484421,2.20672389430872));
#7400=CARTESIAN_POINT('Ctrl Pts',(2.94042729858734,-0.422436975084429,2.36470705955735));
#7401=CARTESIAN_POINT('Ctrl Pts',(1.96067175098405,2.23166560020346,2.52269022480599));
#7402=CARTESIAN_POINT('Ctrl Pts',(-0.797479884797277,2.86157148907721,2.68067339005462));
#7403=CARTESIAN_POINT('Ctrl Pts',(-2.83229010382792,0.895934269397302,2.83865655530326));
#7404=CARTESIAN_POINT('Ctrl Pts',(-2.29811649601273,-1.8823458624239,2.99663972055189));
#7405=CARTESIAN_POINT('Ctrl Pts',(0.320527197372314,-2.95327407483744,3.15462288580053));
#7406=CARTESIAN_POINT('Ctrl Pts',(2.6484417907965,-1.34548188605218,3.31260605104916));
#7407=CARTESIAN_POINT('Ctrl Pts',(2.57412927861735,1.48270829038046,3.47058921629779));
#7408=CARTESIAN_POINT('Ctrl Pts',(0.164993652457452,2.96603144318087,3.62857238154644));
#7409=CARTESIAN_POINT('Ctrl Pts',(-2.3937968492575,1.75906283803822,3.78655554679506));
#7410=CARTESIAN_POINT('Ctrl Pts',(-2.7813319026562,-1.04343580075386,3.94453871204371));
#7411=CARTESIAN_POINT('Ctrl Pts',(-0.646103987851508,-2.89950255412085,
4.10252187729233));
#7412=CARTESIAN_POINT('Ctrl Pts',(2.07516229702079,-2.12562152433648,4.26050504254097));
#7413=CARTESIAN_POINT('Ctrl Pts',(2.91418554866396,0.576270779805192,4.41848820778961));
#7414=CARTESIAN_POINT('Ctrl Pts',(1.10994304032514,2.75546581755331,4.57647137303824));
#7415=CARTESIAN_POINT('Ctrl Pts',(-1.70105569036669,2.43535930845924,4.73445453828687));
#7416=CARTESIAN_POINT('Ctrl Pts',(-2.96913884917045,-0.0937012167956214,
4.8924377035355));
#7417=CARTESIAN_POINT('Ctrl Pts',(-1.54411172877774,-2.53777154140003,5.05042086878415));
#7418=CARTESIAN_POINT('Ctrl Pts',(1.28147743359381,-2.67999645607747,5.20840403403276));
#7419=CARTESIAN_POINT('Ctrl Pts',(2.94472282387208,-0.391373115452234,5.36638719928142));
#7420=CARTESIAN_POINT('Ctrl Pts',(1.93700410367547,2.25223900767807,5.52437036453004));
#7421=CARTESIAN_POINT('Ctrl Pts',(-0.827643453573711,2.85299346104872,5.68235352977868));
#7422=CARTESIAN_POINT('Ctrl Pts',(-2.84159014743252,0.865985497185999,5.84033669502731));
#7423=CARTESIAN_POINT('Ctrl Pts',(-2.27811759136341,-1.90650092936679,5.99831986027594));
#7424=CARTESIAN_POINT('Ctrl Pts',(0.351685383533634,-2.9497258274706,6.15630302552458));
#7425=CARTESIAN_POINT('Ctrl Pts',(2.66249769949282,-1.31744893502235,6.31428619077321));
#7426=CARTESIAN_POINT('Ctrl Pts',(2.55833374879516,1.50979952119754,6.47226935602186));
#7427=CARTESIAN_POINT('Ctrl Pts',(0.133673721473288,2.96760748972438,6.63025252127048));
#7428=CARTESIAN_POINT('Ctrl Pts',(-2.41223284756227,1.73369568500057,6.78823568651912));
#7429=CARTESIAN_POINT('Ctrl Pts',(-2.77016205423848,-1.07274017244211,6.94621885176775));
#7430=CARTESIAN_POINT('Ctrl Pts',(-0.615459410216834,-2.90615854365194,
7.10420201701639));
#7431=CARTESIAN_POINT('Ctrl Pts',(2.09748532109543,-2.10360251662561,7.26218518226503));
#7432=CARTESIAN_POINT('Ctrl Pts',(2.9079404319988,0.60701307178344,7.42016834751365));
#7433=CARTESIAN_POINT('Ctrl Pts',(1.08079210129377,2.76700827096834,7.5781515127623));
#7434=CARTESIAN_POINT('Ctrl Pts',(-1.72666731427814,2.41730681867291,7.73613467801093));
#7435=CARTESIAN_POINT('Ctrl Pts',(-2.96798865827376,-0.125116631992998,
7.89411784325956));
#7436=CARTESIAN_POINT('Ctrl Pts',(-1.51722744668015,-2.55378282744902,8.05210100850819));
#7437=CARTESIAN_POINT('Ctrl Pts',(1.30968108969348,-2.66660189256488,8.21008417375684));
#7438=CARTESIAN_POINT('Ctrl Pts',(2.94872124854132,-0.359724244351702,8.36806733900546));
#7439=CARTESIAN_POINT('Ctrl Pts',(1.91306028218166,2.27152190053491,8.52605050425411));
#7440=CARTESIAN_POINT('Ctrl Pts',(-0.857590960879173,2.84611756069217,8.68403366950273));
#7441=CARTESIAN_POINT('Ctrl Pts',(-2.85088546226824,0.831801059544302,8.84201683475137));
#7442=CARTESIAN_POINT('Ctrl Pts',(-2.45478008065217,-1.00286116724922,8.94733894491712));
#7443=CARTESIAN_POINT('Ctrl Pts',(-1.91346599666504,-1.63598720337498,9.));
#7444=CARTESIAN_POINT('Ctrl Pts',(-1.91346599666504,-1.63598720337498,9.));
#7445=CARTESIAN_POINT('Ctrl Pts',(-1.97510122930192,-1.57806521937354,9.));
#7446=CARTESIAN_POINT('Ctrl Pts',(-2.03336858029506,-1.51699427545506,9.));
#7447=CARTESIAN_POINT('Ctrl Pts',(-2.08826957682143,-1.45315876516108,9.));
#7448=CARTESIAN_POINT('Ctrl Pts',(-2.14462126052521,-1.38763648482453,9.));
#7449=CARTESIAN_POINT('Ctrl Pts',(-2.1974267747986,-1.31920117573619,9.));
#7450=CARTESIAN_POINT('Ctrl Pts',(-2.24666228537762,-1.24821996122214,9.));
#7451=CARTESIAN_POINT('Ctrl Pts',(-2.29723808834736,-1.17530649129776,9.));
#7452=CARTESIAN_POINT('Ctrl Pts',(-2.34404740976649,-1.09970606249909,9.));
#7453=CARTESIAN_POINT('Ctrl Pts',(-2.38703036306917,-1.02177364893372,9.));
#7454=CARTESIAN_POINT('Ctrl Pts',(-2.4059069163696,-0.987548560952,9.));
#7455=CARTESIAN_POINT('Ctrl Pts',(-2.42404501517521,-0.95287321932183,9.));
#7456=CARTESIAN_POINT('Ctrl Pts',(-2.4414371795908,-0.917775628914927,9.));
#7457=CARTESIAN_POINT('Ctrl Pts',(-2.45136171608851,-0.897747798643102,
9.));
#7458=CARTESIAN_POINT('Ctrl Pts',(-2.4610433321017,-0.877582454455379,9.));
#7459=CARTESIAN_POINT('Ctrl Pts',(-2.47048040473327,-0.857284652451543,
9.));
#7460=CARTESIAN_POINT('Ctrl Pts',(-2.4790010742832,-0.838957903234229,9.));
#7461=CARTESIAN_POINT('Ctrl Pts',(-2.48732477223045,-0.820517427059542,
9.));
#7462=CARTESIAN_POINT('Ctrl Pts',(-2.49543660387403,-0.801998763017973,
9.));
#7463=CARTESIAN_POINT('Ctrl Pts',(-2.53203081792429,-0.718457093807081,
9.));
#7464=CARTESIAN_POINT('Ctrl Pts',(-2.56436348011502,-0.63323212592296,9.));
#7465=CARTESIAN_POINT('Ctrl Pts',(-2.5924085980561,-0.546721977487591,9.));
#7466=CARTESIAN_POINT('Ctrl Pts',(-2.62091304129589,-0.458794958570371,
9.));
#7467=CARTESIAN_POINT('Ctrl Pts',(-2.64498884113912,-0.369539561869024,
9.));
#7468=CARTESIAN_POINT('Ctrl Pts',(-2.66456964086263,-0.279336683014174,
9.));
#7469=CARTESIAN_POINT('Ctrl Pts',(-2.68356521302629,-0.191829772221376,
9.));
#7470=CARTESIAN_POINT('Ctrl Pts',(-2.69833062202798,-0.10343025333291,9.));
#7471=CARTESIAN_POINT('Ctrl Pts',(-2.70876448070549,-0.0144639948968432,
9.));
#7472=CARTESIAN_POINT('Ctrl Pts',(-2.71312791197798,0.0227416225314671,
9.));
#7473=CARTESIAN_POINT('Ctrl Pts',(-2.71673328148375,0.0600465487674368,
9.));
#7474=CARTESIAN_POINT('Ctrl Pts',(-2.71957085608624,0.09742756389295,9.));
#7475=CARTESIAN_POINT('Ctrl Pts',(-2.72134533161258,0.120803758630415,9.));
#7476=CARTESIAN_POINT('Ctrl Pts',(-2.72281952388506,0.144209714226741,9.));
#7477=CARTESIAN_POINT('Ctrl Pts',(-2.72399076243517,0.167639784643834,9.));
#7478=CARTESIAN_POINT('Ctrl Pts',(-2.72467743928119,0.181376428519216,9.));
#7479=CARTESIAN_POINT('Ctrl Pts',(-2.72525970776296,0.19511678651136,9.00000000000001));
#7480=CARTESIAN_POINT('Ctrl Pts',(-2.72573704181005,0.208851493316018,9.00000000000001));
#7481=CARTESIAN_POINT('Ctrl Pts',(-2.72911014315679,0.305908383145141,9.00000000000001));
#7482=CARTESIAN_POINT('Ctrl Pts',(-2.72725356321717,0.402803406061901,9.));
#7483=CARTESIAN_POINT('Ctrl Pts',(-2.7201015526238,0.499115315406068,9.));
#7484=CARTESIAN_POINT('Ctrl Pts',(-2.71294954203042,0.595427224750235,9.));
#7485=CARTESIAN_POINT('Ctrl Pts',(-2.70050253761008,0.69115707285682,9.));
#7486=CARTESIAN_POINT('Ctrl Pts',(-2.68264189514795,0.785902555476956,9.));
#7487=CARTESIAN_POINT('Ctrl Pts',(-2.6655684581099,0.876472143641819,9.));
#7488=CARTESIAN_POINT('Ctrl Pts',(-2.64354819167242,0.966143195066629,9.));
#7489=CARTESIAN_POINT('Ctrl Pts',(-2.61685636836744,1.05467578508374,9.));
#7490=CARTESIAN_POINT('Ctrl Pts',(-2.60792497911495,1.08429980191986,9.));
#7491=CARTESIAN_POINT('Ctrl Pts',(-2.59847010448723,1.11379631508768,9.));
#7492=CARTESIAN_POINT('Ctrl Pts',(-2.58850078352238,1.14315615835076,9.));
#7493=CARTESIAN_POINT('Ctrl Pts',(-2.58205201908924,1.16214789446448,9.));
#7494=CARTESIAN_POINT('Ctrl Pts',(-2.57538798275344,1.18108244148084,9.));
#7495=CARTESIAN_POINT('Ctrl Pts',(-2.56851098701296,1.19995728413151,9.));
#7496=CARTESIAN_POINT('Ctrl Pts',(-2.56187356995564,1.21817457076241,9.));
#7497=CARTESIAN_POINT('Ctrl Pts',(-2.55503596749083,1.23634058633936,9.));
#7498=CARTESIAN_POINT('Ctrl Pts',(-2.5480112160171,1.25442550206745,9.));
#7499=CARTESIAN_POINT('Ctrl Pts',(-2.51416429529988,1.34156292053919,9.));
#7500=CARTESIAN_POINT('Ctrl Pts',(-2.47593826775787,1.42692993566585,9.00000000000001));
#7501=CARTESIAN_POINT('Ctrl Pts',(-2.43366482457034,1.51029236193381,9.00000000000001));
#7502=CARTESIAN_POINT('Ctrl Pts',(-2.38981580722589,1.59676179048456,9.00000000000001));
#7503=CARTESIAN_POINT('Ctrl Pts',(-2.34161192708367,1.68107514437489,9.));
#7504=CARTESIAN_POINT('Ctrl Pts',(-2.28936736609892,1.76296811103273,9.));
#7505=CARTESIAN_POINT('Ctrl Pts',(-2.23652986509351,1.84579050682973,9.));
#7506=CARTESIAN_POINT('Ctrl Pts',(-2.1795590352686,1.92613808521401,9.));
#7507=CARTESIAN_POINT('Ctrl Pts',(-2.11872806710601,2.00372262354843,9.));
#7508=CARTESIAN_POINT('Ctrl Pts',(-2.07707869447161,2.0568427274258,9.));
#7509=CARTESIAN_POINT('Ctrl Pts',(-2.0336186907015,2.10866727264771,9.));
#7510=CARTESIAN_POINT('Ctrl Pts',(-1.98842354991113,2.15909672967731,9.));
#7511=CARTESIAN_POINT('Ctrl Pts',(-1.97696960898531,2.17187721916438,9.));
#7512=CARTESIAN_POINT('Ctrl Pts',(-1.96540269677891,2.1845695710529,9.));
#7513=CARTESIAN_POINT('Ctrl Pts',(-1.95373641455615,2.1971589298009,9.));
#7514=CARTESIAN_POINT('Ctrl Pts',(-1.88513603210895,2.27118721133798,9.));
#7515=CARTESIAN_POINT('Ctrl Pts',(-1.81301936191858,2.34175191206966,8.99999999999999));
#7516=CARTESIAN_POINT('Ctrl Pts',(-1.73769803691675,2.4085627715844,9.));
#7517=CARTESIAN_POINT('Ctrl Pts',(-1.67462788387254,2.46450670425561,9.));
#7518=CARTESIAN_POINT('Ctrl Pts',(-1.60930970274182,2.51781862546635,9.));
#7519=CARTESIAN_POINT('Ctrl Pts',(-1.54190247847365,2.56831427040715,9.));
#7520=CARTESIAN_POINT('Ctrl Pts',(-1.50803174514331,2.59368728558025,9.));
#7521=CARTESIAN_POINT('Ctrl Pts',(-1.47363323977049,2.61834899713265,9.));
#7522=CARTESIAN_POINT('Ctrl Pts',(-1.43872534941306,2.64227437840376,9.));
#7523=CARTESIAN_POINT('Ctrl Pts',(-1.42333762902739,2.65282090737903,9.));
#7524=CARTESIAN_POINT('Ctrl Pts',(-1.40785862868675,2.66321904138253,9.));
#7525=CARTESIAN_POINT('Ctrl Pts',(-1.39229155460026,2.67346610734178,9.));
#7526=CARTESIAN_POINT('Ctrl Pts',(-1.30709673728478,2.72954581169518,9.));
#7527=CARTESIAN_POINT('Ctrl Pts',(-1.21925453406997,2.78111212367673,9.));
#7528=CARTESIAN_POINT('Ctrl Pts',(-1.12905379957436,2.82785493889709,9.));
#7529=CARTESIAN_POINT('Ctrl Pts',(-1.04989418514209,2.86887614843616,9.));
#7530=CARTESIAN_POINT('Ctrl Pts',(-0.968917198642337,2.90618241367003,9.));
#7531=CARTESIAN_POINT('Ctrl Pts',(-0.886295500097728,2.93953989917748,9.));
#7532=CARTESIAN_POINT('Ctrl Pts',(-0.856268073332328,2.95166310011376,9.));
#7533=CARTESIAN_POINT('Ctrl Pts',(-0.826023230498369,2.96326448152923,9.));
#7534=CARTESIAN_POINT('Ctrl Pts',(-0.795573338178555,2.97434764200039,9.));
#7535=CARTESIAN_POINT('Ctrl Pts',(-2.52134266056864,-0.000655147898209446,
7.88741669750802));
#7536=CARTESIAN_POINT('Ctrl Pts',(-2.52146223070113,-0.0358370156486364,
7.88965041275853));
#7537=CARTESIAN_POINT('Ctrl Pts',(-2.52078886170416,-0.0710141084424755,
7.89188412800905));
#7538=CARTESIAN_POINT('Ctrl Pts',(-2.51930823234222,-0.106157089457993,
7.89411784325956));
#7539=CARTESIAN_POINT('Ctrl Pts',(-2.48440158774256,-0.93467203047832,7.94677889834244));
#7540=CARTESIAN_POINT('Ctrl Pts',(-2.00081451721136,-1.74422742896367,7.99943995342531));
#7541=CARTESIAN_POINT('Ctrl Pts',(-1.28786955921681,-2.16780830572565,8.05210100850819));
#7542=CARTESIAN_POINT('Ctrl Pts',(-0.574924601222266,-2.59138918248764,
8.10476206359107));
#7543=CARTESIAN_POINT('Ctrl Pts',(0.367378244235608,-2.62899553752626,8.15742311867395));
#7544=CARTESIAN_POINT('Ctrl Pts',(1.11170302677253,-2.26331910701003,8.21008417375683));
#7545=CARTESIAN_POINT('Ctrl Pts',(1.85602780930943,-1.89764267649381,8.26274522883971));
#7546=CARTESIAN_POINT('Ctrl Pts',(2.40237452892538,-1.12868346042275,8.31540628392258));
#7547=CARTESIAN_POINT('Ctrl Pts',(2.50293772767341,-0.305662828239462,8.36806733900546));
#7548=CARTESIAN_POINT('Ctrl Pts',(2.60350092642144,0.517357803943831,8.42072839408834));
#7549=CARTESIAN_POINT('Ctrl Pts',(2.25828060430155,1.39443985223937,8.47338944917123));
#7550=CARTESIAN_POINT('Ctrl Pts',(1.62389523606481,1.92874681974668,8.5260505042541));
#7551=CARTESIAN_POINT('Ctrl Pts',(0.989509867828049,2.463053787254,8.57871155933698));
#7552=CARTESIAN_POINT('Ctrl Pts',(0.0659594534744365,2.65458567397309,8.63137261441985));
#7553=CARTESIAN_POINT('Ctrl Pts',(-0.72803150393389,2.41463220047464,8.68403366950273));
#7554=CARTESIAN_POINT('Ctrl Pts',(-1.5220224613422,2.17467872697621,8.73669472458561));
#7555=CARTESIAN_POINT('Ctrl Pts',(-2.18645396180522,1.50323989326025,8.78935577966849));
#7556=CARTESIAN_POINT('Ctrl Pts',(-2.41964336663271,0.708854919703897,8.84201683475137));
#7557=CARTESIAN_POINT('Ctrl Pts',(-2.48665536097282,0.480571300252128,8.85715012233692));
#7558=CARTESIAN_POINT('Ctrl Pts',(-2.51805435150169,0.242134494478738,8.87228340992247));
#7559=CARTESIAN_POINT('Ctrl Pts',(-2.51592828109546,0.00320694493696498,
8.88741669750802));
#7560=CARTESIAN_POINT('Ctrl Pts',(-0.793799282532843,2.9692229537457,-1.11022302462516E-15));
#7561=CARTESIAN_POINT('Ctrl Pts',(-0.886878369010734,2.93517420813052,-1.08381449128764E-15));
#7562=CARTESIAN_POINT('Ctrl Pts',(-0.977892018175826,2.89636073172584,-1.25693831090626E-15));
#7563=CARTESIAN_POINT('Ctrl Pts',(-1.06663133989414,2.85310975855297,-1.32185928869433E-15));
#7564=CARTESIAN_POINT('Ctrl Pts',(-1.15732372244669,2.80890687612374,-1.38820911016277E-15));
#7565=CARTESIAN_POINT('Ctrl Pts',(-1.24564123287364,2.76006840206767,-1.51535923310734E-15));
#7566=CARTESIAN_POINT('Ctrl Pts',(-1.3313319520912,2.70689814245137,-1.60982338570648E-15));
#7567=CARTESIAN_POINT('Ctrl Pts',(-1.41378112297932,2.65573923211314,-1.70071410446299E-15));
#7568=CARTESIAN_POINT('Ctrl Pts',(-1.49379876348973,2.6005691930734,-9.63096719719295E-16));
#7569=CARTESIAN_POINT('Ctrl Pts',(-1.57112748186993,2.54162859144216,-9.08995101411847E-16));
#7570=CARTESIAN_POINT('Ctrl Pts',(-1.63879011045261,2.49005556501483,-8.6165618539283E-16));
#7571=CARTESIAN_POINT('Ctrl Pts',(-1.70439374270875,2.43559500480107,-1.16765261517047E-15));
#7572=CARTESIAN_POINT('Ctrl Pts',(-1.76774130072772,2.3783953552462,-1.12410081243297E-15));
#7573=CARTESIAN_POINT('Ctrl Pts',(-1.78181886636062,2.36568402357109,-1.11442240681417E-15));
#7574=CARTESIAN_POINT('Ctrl Pts',(-1.79578759750834,2.35283474575188,-1.12368001218868E-15));
#7575=CARTESIAN_POINT('Ctrl Pts',(-1.80962592284842,2.33986750951544,-1.12410081243297E-15));
#7576=CARTESIAN_POINT('Ctrl Pts',(-1.88206109072238,2.27199196023008,-1.12630344429686E-15));
#7577=CARTESIAN_POINT('Ctrl Pts',(-1.95103069838081,2.20079578495377,-1.65761929008765E-15));
#7578=CARTESIAN_POINT('Ctrl Pts',(-2.01629458396089,2.12656832619519,-1.59594559789866E-15));
#7579=CARTESIAN_POINT('Ctrl Pts',(-2.08119360973793,2.05275583837715,-1.53461669442375E-15));
#7580=CARTESIAN_POINT('Ctrl Pts',(-2.14242871756392,1.97594507073483,-1.54117032658774E-15));
#7581=CARTESIAN_POINT('Ctrl Pts',(-2.19972015237435,1.89639377131377,-1.55431223447522E-15));
#7582=CARTESIAN_POINT('Ctrl Pts',(-2.25491823235702,1.81974917334377,-1.56697395406905E-15));
#7583=CARTESIAN_POINT('Ctrl Pts',(-2.30645573607158,1.74055992058549,-1.37357914314464E-15));
#7584=CARTESIAN_POINT('Ctrl Pts',(-2.35403753012578,1.65904287815286,-1.346145417358E-15));
#7585=CARTESIAN_POINT('Ctrl Pts',(-2.37402503340242,1.62480032414432,-1.3346214364962E-15));
#7586=CARTESIAN_POINT('Ctrl Pts',(-2.39331395745324,1.59014691080251,-8.58817840424498E-16));
#7587=CARTESIAN_POINT('Ctrl Pts',(-2.4118798230075,1.55509841026105,-8.32667268468867E-16));
#7588=CARTESIAN_POINT('Ctrl Pts',(-2.42490921652519,1.53050161974646,-8.1431498148677E-16));
#7589=CARTESIAN_POINT('Ctrl Pts',(-2.43758246139463,1.50571024066321,-9.02295645932798E-16));
#7590=CARTESIAN_POINT('Ctrl Pts',(-2.44989061107463,1.4807297179593,-8.74300631892311E-16));
#7591=CARTESIAN_POINT('Ctrl Pts',(-2.45765251973512,1.46497620987237,-8.56646090179653E-16));
#7592=CARTESIAN_POINT('Ctrl Pts',(-2.46527012151294,1.44914532838183,-1.01327467154504E-15));
#7593=CARTESIAN_POINT('Ctrl Pts',(-2.47273147665068,1.4332596231852,-1.01307850997046E-15));
#7594=CARTESIAN_POINT('Ctrl Pts',(-2.51485688189898,1.34357192481016,-1.01197101868087E-15));
#7595=CARTESIAN_POINT('Ctrl Pts',(-2.55207895507421,1.25199537848123,-1.57756955155647E-15));
#7596=CARTESIAN_POINT('Ctrl Pts',(-2.58410579009646,1.15880114788537,-1.55431223447522E-15));
#7597=CARTESIAN_POINT('Ctrl Pts',(-2.61396690786283,1.07190889352943,-1.53262762268606E-15));
#7598=CARTESIAN_POINT('Ctrl Pts',(-2.63931147777468,0.98360954884976,-7.90704564077518E-16));
#7599=CARTESIAN_POINT('Ctrl Pts',(-2.65985235348906,0.894114165208975,-7.49400541621981E-16));
#7600=CARTESIAN_POINT('Ctrl Pts',(-2.66134210780213,0.887623393557723,-7.46404912494191E-16));
#7601=CARTESIAN_POINT('Ctrl Pts',(-2.66280657151596,0.881126329458841,-1.17195010629658E-15));
#7602=CARTESIAN_POINT('Ctrl Pts',(-2.66424562422382,0.874623053092889,-1.16573417585641E-15));
#7603=CARTESIAN_POINT('Ctrl Pts',(-2.68482996036177,0.781599617617434,-1.04692289900001E-15));
#7604=CARTESIAN_POINT('Ctrl Pts',(-2.70021925475279,0.687304125014347,-9.81473364557526E-16));
#7605=CARTESIAN_POINT('Ctrl Pts',(-2.71049072825162,0.592145729463149,-8.60422844084496E-16));
#7606=CARTESIAN_POINT('Ctrl Pts',(-2.71630566600268,0.538274184481477,-7.91893120343947E-16));
#7607=CARTESIAN_POINT('Ctrl Pts',(-2.72047941991799,0.484126269723892,-1.33893866460458E-15));
#7608=CARTESIAN_POINT('Ctrl Pts',(-2.72301911106579,0.429778916423232,-1.33226762955019E-15));
#7609=CARTESIAN_POINT('Ctrl Pts',(-2.72366582651429,0.415939724600469,-1.330568894871E-15));
#7610=CARTESIAN_POINT('Ctrl Pts',(-2.72420643309896,0.402088998021608,-1.4283520817037E-15));
#7611=CARTESIAN_POINT('Ctrl Pts',(-2.72464086766462,0.388240253329536,-1.41553435639707E-15));
#7612=CARTESIAN_POINT('Ctrl Pts',(-2.72756562491765,0.295005921429125,-1.32924118817005E-15));
#7613=CARTESIAN_POINT('Ctrl Pts',(-2.72569020906838,0.201710259987124,-1.06406896392454E-15));
#7614=CARTESIAN_POINT('Ctrl Pts',(-2.71914970277427,0.108729654609856,-1.0547118733939E-15));
#7615=CARTESIAN_POINT('Ctrl Pts',(-2.71259881332269,0.0156014410469117,
-1.04533992833364E-15));
#7616=CARTESIAN_POINT('Ctrl Pts',(-2.7013676305465,-0.0772116972142303,
-1.39298541692603E-15));
#7617=CARTESIAN_POINT('Ctrl Pts',(-2.68554097073859,-0.169319449958644,
-1.38777878078145E-15));
#7618=CARTESIAN_POINT('Ctrl Pts',(-2.66994267605977,-0.260098166816704,
-1.38264727193154E-15));
#7619=CARTESIAN_POINT('Ctrl Pts',(-2.64988010285609,-0.35019255259287,-1.0308343657274E-15));
#7620=CARTESIAN_POINT('Ctrl Pts',(-2.62539147593809,-0.439203699437016,
-8.88178419700125E-16));
#7621=CARTESIAN_POINT('Ctrl Pts',(-2.61615129561636,-0.472789863750656,
-8.34350711447145E-16));
#7622=CARTESIAN_POINT('Ctrl Pts',(-2.60628055155745,-0.506221478197271,
-1.63486821342447E-15));
#7623=CARTESIAN_POINT('Ctrl Pts',(-2.59577987598867,-0.539475785607662,
-1.63757896132211E-15));
#7624=CARTESIAN_POINT('Ctrl Pts',(-2.58810257712511,-0.563788817166238,
-1.63956085492672E-15));
#7625=CARTESIAN_POINT('Ctrl Pts',(-2.58008853706366,-0.588007054833637,
-1.58037810929509E-15));
#7626=CARTESIAN_POINT('Ctrl Pts',(-2.57173775820317,-0.612121310772716,
-1.60982338570648E-15));
#7627=CARTESIAN_POINT('Ctrl Pts',(-2.56654706379232,-0.627110299897659,
-1.62812604157221E-15));
#7628=CARTESIAN_POINT('Ctrl Pts',(-2.5612292056814,-0.642050561982069,-1.68622661660371E-15));
#7629=CARTESIAN_POINT('Ctrl Pts',(-2.55578549619449,-0.656937632559102,
-1.69309011255336E-15));
#7630=CARTESIAN_POINT('Ctrl Pts',(-2.52407271214207,-0.743663504966145,
-1.73307398116711E-15));
#7631=CARTESIAN_POINT('Ctrl Pts',(-2.48808276034648,-0.828614815980182,
-9.77241205803787E-16));
#7632=CARTESIAN_POINT('Ctrl Pts',(-2.44787616909233,-0.911389584879519,
-1.22124532708767E-15));
#7633=CARTESIAN_POINT('Ctrl Pts',(-2.41772122565171,-0.973470661554021,
-1.40424841805059E-15));
#7634=CARTESIAN_POINT('Ctrl Pts',(-2.38519343314366,-1.03432694837566,-1.06885018652311E-15));
#7635=CARTESIAN_POINT('Ctrl Pts',(-2.35030323620402,-1.09377384664802,-1.16573417585641E-15));
#7636=CARTESIAN_POINT('Ctrl Pts',(-2.33453826171165,-1.12063465332491,-1.20951075938217E-15));
#7637=CARTESIAN_POINT('Ctrl Pts',(-2.31829080415985,-1.14720751443845,-1.51219465577998E-15));
#7638=CARTESIAN_POINT('Ctrl Pts',(-2.3015610494714,-1.17347433375359,-1.60982338570648E-15));
#7639=CARTESIAN_POINT('Ctrl Pts',(-2.2924218706108,-1.18782344790922,-1.66315629114043E-15));
#7640=CARTESIAN_POINT('Ctrl Pts',(-2.28314390690011,-1.20207312067747,-1.37933724003994E-15));
#7641=CARTESIAN_POINT('Ctrl Pts',(-2.27372792141341,-1.21622019271053,-1.33226762955019E-15));
#7642=CARTESIAN_POINT('Ctrl Pts',(-2.2261576244293,-1.2876923098902,-1.09446826663856E-15));
#7643=CARTESIAN_POINT('Ctrl Pts',(-2.17506395390716,-1.35655363510998,-6.67815194483028E-16));
#7644=CARTESIAN_POINT('Ctrl Pts',(-2.1204781354577,-1.42244994398426,-2.77555756156289E-16));
#7645=CARTESIAN_POINT('Ctrl Pts',(-2.07432924150386,-1.47816114987198,5.23841796256794E-17));
#7646=CARTESIAN_POINT('Ctrl Pts',(-2.02568360871182,-1.53175271241673,-1.28432281748436E-16));
#7647=CARTESIAN_POINT('Ctrl Pts',(-1.97454380027699,-1.58298639353747,-1.66533453693773E-16));
#7648=CARTESIAN_POINT('Ctrl Pts',(-1.9557112793937,-1.60185348356312,-6.86465273718822E-17));
#7649=CARTESIAN_POINT('Ctrl Pts',(-1.93654037332315,-1.62040056709866,1.19381178188368E-16));
#7650=CARTESIAN_POINT('Ctrl Pts',(-1.91704123069774,-1.63862336360398,1.11022302462516E-16));
#7651=CARTESIAN_POINT('Origin',(0.,0.,9.));
#7652=CARTESIAN_POINT('',(-7.,-8.57252759403147E-16,9.));
#7653=CARTESIAN_POINT('Origin',(0.,0.,9.));
#7654=CARTESIAN_POINT('Origin',(0.,0.,4.));
#7655=CARTESIAN_POINT('',(-7.,-8.57252759403147E-16,4.));
#7656=CARTESIAN_POINT('Origin',(0.,0.,4.));
#7657=CARTESIAN_POINT('',(-5.,-6.12323399573677E-16,4.));
#7658=CARTESIAN_POINT('Origin',(0.,0.,4.));
#7659=CARTESIAN_POINT('Origin',(0.,0.,2.));
#7660=CARTESIAN_POINT('',(-7.,-8.57252759403147E-16,2.));
#7661=CARTESIAN_POINT('Origin',(0.,0.,2.));
#7662=CARTESIAN_POINT('',(-5.,6.12323399573677E-16,2.));
#7663=CARTESIAN_POINT('Origin',(0.,0.,2.));
#7664=CARTESIAN_POINT('Origin',(0.,0.,2.));
#7665=CARTESIAN_POINT('',(-7.,-8.57252759403147E-16,2.));
#7666=CARTESIAN_POINT('Origin',(0.,0.,0.));
#7667=CARTESIAN_POINT('',(-5.,-6.12323399573677E-16,0.));
#7668=CARTESIAN_POINT('',(-5.,-6.12323399573677E-16,0.));
#7669=CARTESIAN_POINT('Origin',(0.,0.,0.));
#7670=CARTESIAN_POINT('Origin',(0.,0.,8.));
#7671=CARTESIAN_POINT('',(-7.,-8.57252759403147E-16,8.));
#7672=CARTESIAN_POINT('Origin',(0.,0.,8.));
#7673=CARTESIAN_POINT('',(-5.,-6.12323399573677E-16,8.));
#7674=CARTESIAN_POINT('Origin',(0.,0.,8.));
#7675=CARTESIAN_POINT('Origin',(0.,0.,8.));
#7676=CARTESIAN_POINT('',(-7.,-8.57252759403147E-16,8.));
#7677=CARTESIAN_POINT('Origin',(0.,0.,0.));
#7678=CARTESIAN_POINT('Origin',(0.,0.,0.));
#7679=CARTESIAN_POINT('',(-5.,-6.12323399573677E-16,0.));
#7680=CARTESIAN_POINT('Origin',(0.,0.,0.));
#7681=CARTESIAN_POINT('',(0.,0.,0.));
#7682=CARTESIAN_POINT('Origin',(0.,0.,0.));
#7683=CARTESIAN_POINT('',(-2.94437861999191,0.00228824954296311,0.322176117089596));
#7684=CARTESIAN_POINT('',(-2.94436911647834,0.00312614869137163,0.177823882910396));
#7685=CARTESIAN_POINT('',(-2.942,-3.60291088309151E-16,0.));
#7686=CARTESIAN_POINT('',(1.28892185405323,2.64462557919717,0.));
#7687=CARTESIAN_POINT('Ctrl Pts',(-2.94437861999191,0.00228824954296311,
0.322176117089596));
#7688=CARTESIAN_POINT('Ctrl Pts',(-2.94551635113874,0.142778583613822,0.314557432409286));
#7689=CARTESIAN_POINT('Ctrl Pts',(-2.93631267309395,0.283111895578672,0.306938747728977));
#7690=CARTESIAN_POINT('Ctrl Pts',(-2.91624915612822,0.42186500989966,0.299320063048668));
#7691=CARTESIAN_POINT('Ctrl Pts',(-2.77830971889191,1.37581174500659,0.246940558544163));
#7692=CARTESIAN_POINT('Ctrl Pts',(-2.1270526803082,2.25506646395135,0.194561054039658));
#7693=CARTESIAN_POINT('Ctrl Pts',(-1.25475282359973,2.66583045735473,0.142181549535154));
#7694=CARTESIAN_POINT('Ctrl Pts',(-0.46548135530728,3.03749657388775,0.0947876996901026));
#7695=CARTESIAN_POINT('Ctrl Pts',(0.504756374147381,3.02561249996607,0.0473938498450515));
#7696=CARTESIAN_POINT('Ctrl Pts',(1.29197400994443,2.64783394680711,3.05745012640912E-16));
#7697=CARTESIAN_POINT('',(-1.28892185405326,2.64462557919716,0.));
#7698=CARTESIAN_POINT('Origin',(0.,0.,0.));
#7699=CARTESIAN_POINT('Ctrl Pts',(-1.28892185405326,2.64462557919716,1.87350135405495E-15));
#7700=CARTESIAN_POINT('Ctrl Pts',(-2.16038499609478,2.21989706654312,0.0524451052237091));
#7701=CARTESIAN_POINT('Ctrl Pts',(-2.79846764402885,1.33473338532309,0.104890210447416));
#7702=CARTESIAN_POINT('Ctrl Pts',(-2.92193100282573,0.379041548713593,0.157335315671123));
#7703=CARTESIAN_POINT('Ctrl Pts',(-2.93800868581449,0.25458915624929,0.164164838084214));
#7704=CARTESIAN_POINT('Ctrl Pts',(-2.94535953294187,0.128940758021734,0.170994360497305));
#7705=CARTESIAN_POINT('Ctrl Pts',(-2.94436911647834,0.00312614869137163,
0.177823882910396));
#7706=CARTESIAN_POINT('Origin',(0.,0.,0.));
#7707=CARTESIAN_POINT('',(-2.93740032720055,-0.000139020310086779,1.32217611708959));
#7708=CARTESIAN_POINT('',(-2.93737720095951,0.000230872487724698,1.1778238829104));
#7709=CARTESIAN_POINT('',(-2.942,-3.60291088309151E-16,0.));
#7710=CARTESIAN_POINT('Ctrl Pts',(-2.93740032720055,-0.000139020310086779,
1.32217611708959));
#7711=CARTESIAN_POINT('Ctrl Pts',(-2.93718361365059,0.494770241727901,1.29550112610298));
#7712=CARTESIAN_POINT('Ctrl Pts',(-2.81848923912434,0.989776479202536,1.26882613511636));
#7713=CARTESIAN_POINT('Ctrl Pts',(-2.58191143461274,1.4199490257311,1.24215114412975));
#7714=CARTESIAN_POINT('Ctrl Pts',(-2.11736289237333,2.26464377557798,1.18977163962524));
#7715=CARTESIAN_POINT('Ctrl Pts',(-1.19827972440715,2.85935294685526,1.13739213512074));
#7716=CARTESIAN_POINT('Ctrl Pts',(-0.2374000875181,2.93702585155106,1.08501263061624));
#7717=CARTESIAN_POINT('Ctrl Pts',(0.723479549370952,3.01469875624685,1.03263312611173));
#7718=CARTESIAN_POINT('Ctrl Pts',(1.72615565518287,2.57533539436116,0.980253621607226));
#7719=CARTESIAN_POINT('Ctrl Pts',(2.32033868002489,1.8162041612206,0.927874117102722));
#7720=CARTESIAN_POINT('Ctrl Pts',(2.9145217048669,1.05707292808004,0.875494612598217));
#7721=CARTESIAN_POINT('Ctrl Pts',(3.100211648739,-0.0218261763153739,0.823115108093712));
#7722=CARTESIAN_POINT('Ctrl Pts',(2.79403320730894,-0.935902477435646,0.770735603589208));
#7723=CARTESIAN_POINT('Ctrl Pts',(2.48785476587888,-1.84997877855592,0.718356099084703));
#7724=CARTESIAN_POINT('Ctrl Pts',(1.68980793914667,-2.59923227640105,0.665976594580199));
#7725=CARTESIAN_POINT('Ctrl Pts',(0.75825229618776,-2.84733793424016,0.613597090075694));
#7726=CARTESIAN_POINT('Ctrl Pts',(-0.173303346771145,-3.09544359207927,
0.56121758557119));
#7727=CARTESIAN_POINT('Ctrl Pts',(-1.23836780595674,-2.84240140991237,0.508838081066685));
#7728=CARTESIAN_POINT('Ctrl Pts',(-1.95858911760509,-2.20156094319437,0.456458576562181));
#7729=CARTESIAN_POINT('Ctrl Pts',(-2.57405306040479,-1.65393177147606,0.411697756737986));
#7730=CARTESIAN_POINT('Ctrl Pts',(-2.93769429310237,-0.823111776086056,
0.366936936913791));
#7731=CARTESIAN_POINT('Ctrl Pts',(-2.94437861999191,0.00228824954296311,
0.322176117089596));
#7732=CARTESIAN_POINT('Ctrl Pts',(-2.94436911647834,0.00312614869137163,
0.177823882910396));
#7733=CARTESIAN_POINT('Ctrl Pts',(-2.93775395051561,-0.837211781775621,
0.223439465721013));
#7734=CARTESIAN_POINT('Ctrl Pts',(-2.55902339432207,-1.68496462111194,0.26905504853163));
#7735=CARTESIAN_POINT('Ctrl Pts',(-1.92306539600717,-2.23328718212897,0.314670631342247));
#7736=CARTESIAN_POINT('Ctrl Pts',(-1.19189236073203,-2.86370408436305,0.367115736565955));
#7737=CARTESIAN_POINT('Ctrl Pts',(-0.120702220522052,-3.09831789683223,
0.419560841789662));
#7738=CARTESIAN_POINT('Ctrl Pts',(0.807638005699694,-2.8335361097114,0.47200594701337));
#7739=CARTESIAN_POINT('Ctrl Pts',(1.73597823192144,-2.56875432259058,0.524451052237078));
#7740=CARTESIAN_POINT('Ctrl Pts',(2.52146854415495,-1.80457693587975,0.576896157460787));
#7741=CARTESIAN_POINT('Ctrl Pts',(2.81091642121069,-0.883954119006901,0.629341262684494));
#7742=CARTESIAN_POINT('Ctrl Pts',(3.10036429826643,0.0366686978659464,0.681786367908202));
#7743=CARTESIAN_POINT('Ctrl Pts',(2.89376974014439,1.11373694490081,0.734231473131909));
#7744=CARTESIAN_POINT('Ctrl Pts',(2.28393241469019,1.86192138048068,0.786676578355617));
#7745=CARTESIAN_POINT('Ctrl Pts',(1.674095089236,2.61010581606054,0.839121683579324));
#7746=CARTESIAN_POINT('Ctrl Pts',(0.661014996449636,3.02940644018541,0.891566788803033));
#7747=CARTESIAN_POINT('Ctrl Pts',(-0.299207810136722,2.93136603044105,0.944011894026741));
#7748=CARTESIAN_POINT('Ctrl Pts',(-1.25943061672308,2.83332562069669,0.996456999250449));
#7749=CARTESIAN_POINT('Ctrl Pts',(-2.16679613710945,2.21794417708309,1.04890210447416));
#7750=CARTESIAN_POINT('Ctrl Pts',(-2.61293993368518,1.36206873790977,1.10134720969786));
#7751=CARTESIAN_POINT('Ctrl Pts',(-2.82979902340055,0.946049575313678,1.12683943410204));
#7752=CARTESIAN_POINT('Ctrl Pts',(-2.93768601866802,0.47320929383844,1.15233165850622));
#7753=CARTESIAN_POINT('Ctrl Pts',(-2.93737720095951,0.000230872487724698,
1.1778238829104));
#7754=CARTESIAN_POINT('Origin',(0.,0.,0.));
#7755=CARTESIAN_POINT('',(-2.94487182720719,-0.00190539986535287,2.32217611708959));
#7756=CARTESIAN_POINT('',(-2.94409804542743,-0.00221960462873976,2.1778238829104));
#7757=CARTESIAN_POINT('',(-2.942,-3.60291088309151E-16,0.));
#7758=CARTESIAN_POINT('Ctrl Pts',(-2.94487182720719,-0.00190539986535287,
2.32217611708959));
#7759=CARTESIAN_POINT('Ctrl Pts',(-2.93849254859689,0.841069663508672,2.27644481979667));
#7760=CARTESIAN_POINT('Ctrl Pts',(-2.55692453936773,1.68909389771769,2.23071352250375));
#7761=CARTESIAN_POINT('Ctrl Pts',(-1.91797659724234,2.23693579382214,2.18498222521083));
#7762=CARTESIAN_POINT('Ctrl Pts',(-1.18614132044426,2.86442044357863,2.13260272070633));
#7763=CARTESIAN_POINT('Ctrl Pts',(-0.116653199765081,3.09810042098425,2.08022321620182));
#7764=CARTESIAN_POINT('Ctrl Pts',(0.810201861614963,2.83303510458914,2.02784371169732));
#7765=CARTESIAN_POINT('Ctrl Pts',(1.73705692299501,2.56796978819403,1.97546420719281));
#7766=CARTESIAN_POINT('Ctrl Pts',(2.52127892507592,1.80415917799819,1.92308470268831));
#7767=CARTESIAN_POINT('Ctrl Pts',(2.81068910755427,0.88461468761641,1.8707051981838));
#7768=CARTESIAN_POINT('Ctrl Pts',(3.10009929003262,-0.0349298027653776,
1.8183256936793));
#7769=CARTESIAN_POINT('Ctrl Pts',(2.89469765290841,-1.11020817333311,1.76594618917479));
#7770=CARTESIAN_POINT('Ctrl Pts',(2.28672630753671,-1.85833254788295,1.71356668467029));
#7771=CARTESIAN_POINT('Ctrl Pts',(1.67875496216501,-2.60645692243279,1.66118718016578));
#7772=CARTESIAN_POINT('Ctrl Pts',(0.668213908545816,-3.02742730096473,1.60880767566128));
#7773=CARTESIAN_POINT('Ctrl Pts',(-0.291083395731117,-2.93219727380604,
1.55642817115678));
#7774=CARTESIAN_POINT('Ctrl Pts',(-1.25038070000804,-2.83696724664735,1.50404866665227));
#7775=CARTESIAN_POINT('Ctrl Pts',(-2.15843425494271,-2.22553681379804,1.45166916214777));
#7776=CARTESIAN_POINT('Ctrl Pts',(-2.60745407415374,-1.37248143316515,1.39928965764326));
#7777=CARTESIAN_POINT('Ctrl Pts',(-2.82780430697652,-0.953856366540085,
1.37358514412537));
#7778=CARTESIAN_POINT('Ctrl Pts',(-2.93760915637607,-0.477042717206063,
1.34788063060748));
#7779=CARTESIAN_POINT('Ctrl Pts',(-2.93740032720055,-0.000139020310086779,
1.32217611708959));
#7780=CARTESIAN_POINT('Ctrl Pts',(-2.93737720095951,0.000230872487724698,
1.1778238829104));
#7781=CARTESIAN_POINT('Ctrl Pts',(-2.9370506885783,-0.499848321024544,1.20477676372993));
#7782=CARTESIAN_POINT('Ctrl Pts',(-2.81577431600542,-1.00008193824477,1.23172964454946));
#7783=CARTESIAN_POINT('Ctrl Pts',(-2.57446559490686,-1.43347457044749,1.25868252536899));
#7784=CARTESIAN_POINT('Ctrl Pts',(-2.10492538678771,-2.27677300489839,1.31112763059269));
#7785=CARTESIAN_POINT('Ctrl Pts',(-1.1809228977843,-2.86700043906715,1.3635727358164));
#7786=CARTESIAN_POINT('Ctrl Pts',(-0.218377608724914,-2.93852741234213,
1.41601784104011));
#7787=CARTESIAN_POINT('Ctrl Pts',(0.744167680334467,-3.01005438561711,1.46846294626382));
#7788=CARTESIAN_POINT('Ctrl Pts',(1.74525576944982,-2.56288089799832,1.52090805148753));
#7789=CARTESIAN_POINT('Ctrl Pts',(2.33429173832943,-1.79826479808332,1.57335315671123));
#7790=CARTESIAN_POINT('Ctrl Pts',(2.92332770720905,-1.03364869816832,1.62579826193494));
#7791=CARTESIAN_POINT('Ctrl Pts',(3.10031155585293,0.0484100140428809,1.67824336715865));
#7792=CARTESIAN_POINT('Ctrl Pts',(2.78557670999694,0.960852278151669,1.73068847238236));
#7793=CARTESIAN_POINT('Ctrl Pts',(2.47084186414094,1.87329454226046,1.78313357760607));
#7794=CARTESIAN_POINT('Ctrl Pts',(1.66438832378506,2.61612035826684,1.83557868282977));
#7795=CARTESIAN_POINT('Ctrl Pts',(0.729213057861966,2.85498007465664,1.88802378805348));
#7796=CARTESIAN_POINT('Ctrl Pts',(-0.205962208061124,3.09383979104644,1.94046889327719));
#7797=CARTESIAN_POINT('Ctrl Pts',(-1.26985919955142,2.82873340781965,1.9929139985009));
#7798=CARTESIAN_POINT('Ctrl Pts',(-1.98360551176881,2.17898571169394,2.0453591037246));
#7799=CARTESIAN_POINT('Ctrl Pts',(-2.58452748049057,1.63194587688865,2.08951403011987));
#7800=CARTESIAN_POINT('Ctrl Pts',(-2.93724853244873,0.81225677381718,2.13366895651513));
#7801=CARTESIAN_POINT('Ctrl Pts',(-2.94409804542743,-0.00221960462873976,
2.1778238829104));
#7802=CARTESIAN_POINT('Origin',(0.,0.,0.));
#7803=CARTESIAN_POINT('',(-2.94188729812012,0.00254759896953657,3.32217611708959));
#7804=CARTESIAN_POINT('',(-2.94300132914192,0.00247067809074119,3.17782388291039));
#7805=CARTESIAN_POINT('',(-2.942,-3.60291088309151E-16,0.));
#7806=CARTESIAN_POINT('Ctrl Pts',(-2.94188729812012,0.00254759896953657,
3.32217611708959));
#7807=CARTESIAN_POINT('Ctrl Pts',(-2.94391723822425,0.231870355671395,3.30976801799487));
#7808=CARTESIAN_POINT('Ctrl Pts',(-2.91930872547992,0.460762551320829,3.29735991890015));
#7809=CARTESIAN_POINT('Ctrl Pts',(-2.86638309031571,0.682908266801983,3.28495181980542));
#7810=CARTESIAN_POINT('Ctrl Pts',(-2.64296300603654,1.62067338423639,3.23257231530092));
#7811=CARTESIAN_POINT('Ctrl Pts',(-1.91492649555138,2.438214961245,3.18019281079642));
#7812=CARTESIAN_POINT('Ctrl Pts',(-1.00922037183541,2.76839122410029,3.12781330629191));
#7813=CARTESIAN_POINT('Ctrl Pts',(-0.103514248119433,3.09856748695557,3.07543380178741));
#7814=CARTESIAN_POINT('Ctrl Pts',(0.979861488827348,2.94137843565753,3.0230542972829));
#7815=CARTESIAN_POINT('Ctrl Pts',(1.75438420282982,2.3674145763557,2.9706747927784));
#7816=CARTESIAN_POINT('Ctrl Pts',(2.5289069168323,1.79345071705387,2.91829528827389));
#7817=CARTESIAN_POINT('Ctrl Pts',(2.99457660789046,0.802712049748258,2.86591578376939));
#7818=CARTESIAN_POINT('Ctrl Pts',(2.94227021542597,-0.159880282562335,2.81353627926488));
#7819=CARTESIAN_POINT('Ctrl Pts',(2.88996382296149,-1.12247261487293,2.76115677476038));
#7820=CARTESIAN_POINT('Ctrl Pts',(2.31968134697434,-2.0569186121885,2.70877727025587));
#7821=CARTESIAN_POINT('Ctrl Pts',(1.48752538566269,-2.54357700727495,2.65639776575137));
#7822=CARTESIAN_POINT('Ctrl Pts',(0.655369424351043,-3.0302354023614,2.60401826124687));
#7823=CARTESIAN_POINT('Ctrl Pts',(-0.438660022285117,-3.06910619521874,
2.55163875674236));
#7824=CARTESIAN_POINT('Ctrl Pts',(-1.30325595742871,-2.64273334365957,2.49925925223786));
#7825=CARTESIAN_POINT('Ctrl Pts',(-2.1678518925723,-2.21636049210041,2.44687974773335));
#7826=CARTESIAN_POINT('Ctrl Pts',(-2.80301431622333,-1.32474399612474,2.39450024322885));
#7827=CARTESIAN_POINT('Ctrl Pts',(-2.92350431159035,-0.368291087083228,
2.34212073872434));
#7828=CARTESIAN_POINT('Ctrl Pts',(-2.93879736301763,-0.246894422727957,
2.33547253151276));
#7829=CARTESIAN_POINT('Ctrl Pts',(-2.94579921760659,-0.124453265927633,
2.32882432430118));
#7830=CARTESIAN_POINT('Ctrl Pts',(-2.94487182720719,-0.00190539986535287,
2.32217611708959));
#7831=CARTESIAN_POINT('Ctrl Pts',(-2.94409804542743,-0.00221960462873976,
2.1778238829104));
#7832=CARTESIAN_POINT('Ctrl Pts',(-2.94538405566721,-0.155139230593375,
2.18611406173884));
#7833=CARTESIAN_POINT('Ctrl Pts',(-2.93447780370748,-0.307875103637501,
2.19440424056728));
#7834=CARTESIAN_POINT('Ctrl Pts',(-2.91073286453113,-0.458588216909009,
2.20269441939573));
#7835=CARTESIAN_POINT('Ctrl Pts',(-2.76051827213159,-1.41202544036162,2.25513952461944));
#7836=CARTESIAN_POINT('Ctrl Pts',(-2.09649345438802,-2.28451087824219,2.30758462984315));
#7837=CARTESIAN_POINT('Ctrl Pts',(-1.21754466145652,-2.68332862013697,2.36002973506685));
#7838=CARTESIAN_POINT('Ctrl Pts',(-0.338595868525027,-3.08214636203174,
2.41247484029056));
#7839=CARTESIAN_POINT('Ctrl Pts',(0.755276899594388,-3.00729640794073,2.46491994551426));
#7840=CARTESIAN_POINT('Ctrl Pts',(1.57170784623814,-2.49246924635079,2.51736505073797));
#7841=CARTESIAN_POINT('Ctrl Pts',(2.3881387928819,-1.97764208476085,2.56981015596168));
#7842=CARTESIAN_POINT('Ctrl Pts',(2.92712791805,-1.02283771567197,2.62225526118539));
#7843=CARTESIAN_POINT('Ctrl Pts',(2.94606932856971,-0.0578258660348382,
2.6747003664091));
#7844=CARTESIAN_POINT('Ctrl Pts',(2.96501073908941,0.907185983602299,2.72714547163281));
#7845=CARTESIAN_POINT('Ctrl Pts',(2.46390443496074,1.88240531378769,2.77959057685651));
#7846=CARTESIAN_POINT('Ctrl Pts',(1.66830473495772,2.42887370127543,2.83203568208022));
#7847=CARTESIAN_POINT('Ctrl Pts',(0.872705034954712,2.97534208876317,2.88448078730393));
#7848=CARTESIAN_POINT('Ctrl Pts',(-0.217388060922636,3.09305953355326,2.93692589252764));
#7849=CARTESIAN_POINT('Ctrl Pts',(-1.11130990317228,2.72903986659667,2.98937099775135));
#7850=CARTESIAN_POINT('Ctrl Pts',(-2.00523174542191,2.36502019964009,3.04181610297505));
#7851=CARTESIAN_POINT('Ctrl Pts',(-2.70298233404385,1.51926342093683,3.09426120819876));
#7852=CARTESIAN_POINT('Ctrl Pts',(-2.89049530439613,0.572455370821353,3.14670631342247));
#7853=CARTESIAN_POINT('Ctrl Pts',(-2.92758137029262,0.385196933861252,3.15707883658511));
#7854=CARTESIAN_POINT('Ctrl Pts',(-2.94470877622731,0.1939857347123,3.16745135974775));
#7855=CARTESIAN_POINT('Ctrl Pts',(-2.94300132914192,0.00247067809074119,
3.17782388291039));
#7856=CARTESIAN_POINT('Origin',(0.,0.,0.));
#7857=CARTESIAN_POINT('',(-2.93815144027097,-0.00144838940242836,4.32217611708959));
#7858=CARTESIAN_POINT('',(-2.93758805006728,-0.000810565913221897,4.1778238829104));
#7859=CARTESIAN_POINT('',(-2.942,-3.60291088309151E-16,0.));
#7860=CARTESIAN_POINT('Ctrl Pts',(-2.93815144027097,-0.00144838940242836,
4.32217611708959));
#7861=CARTESIAN_POINT('Ctrl Pts',(-2.93549507201127,0.581944663119171,4.29071171168856));
#7862=CARTESIAN_POINT('Ctrl Pts',(-2.76704590305946,1.16675179323199,4.25924730628754));
#7863=CARTESIAN_POINT('Ctrl Pts',(-2.44338137442995,1.64693751569171,4.22778290088651));
#7864=CARTESIAN_POINT('Ctrl Pts',(-1.90456974207211,2.44631350554451,4.175403396382));
#7865=CARTESIAN_POINT('Ctrl Pts',(-0.93560961338887,2.95575207374732,4.1230238918775));
#7866=CARTESIAN_POINT('Ctrl Pts',(0.0283581627927666,2.94647442485208,4.07064438737299));
#7867=CARTESIAN_POINT('Ctrl Pts',(0.992325938974403,2.93719677595684,4.01826488286848));
#7868=CARTESIAN_POINT('Ctrl Pts',(1.95130136265442,2.40920290996356,3.96588537836398));
#7869=CARTESIAN_POINT('Ctrl Pts',(2.4746275187937,1.59960444002515,3.91350587385948));
#7870=CARTESIAN_POINT('Ctrl Pts',(2.99795367493297,0.790005970086747,3.86112636935497));
#7871=CARTESIAN_POINT('Ctrl Pts',(3.0856305635315,-0.301197103796779,3.80874686485047));
#7872=CARTESIAN_POINT('Ctrl Pts',(2.69828422619929,-1.18396704178881,3.75636736034596));
#7873=CARTESIAN_POINT('Ctrl Pts',(2.31093788886708,-2.06673697978085,3.70398785584146));
#7874=CARTESIAN_POINT('Ctrl Pts',(1.44856832560414,-2.7410737818814,3.65160835133695));
#7875=CARTESIAN_POINT('Ctrl Pts',(0.498448668458934,-2.90414611332682,3.59922884683245));
#7876=CARTESIAN_POINT('Ctrl Pts',(-0.451670988686273,-3.06721844477224,
3.54684934232795));
#7877=CARTESIAN_POINT('Ctrl Pts',(-1.48954073971375,-2.71902630556253,3.49446983782344));
#7878=CARTESIAN_POINT('Ctrl Pts',(-2.1490737861909,-2.01593590702758,3.44209033331894));
#7879=CARTESIAN_POINT('Ctrl Pts',(-2.65237107835254,-1.47939949597489,3.40211892790916));
#7880=CARTESIAN_POINT('Ctrl Pts',(-2.93534805643284,-0.736191897535303,
3.36214752249938));
#7881=CARTESIAN_POINT('Ctrl Pts',(-2.94188729812012,0.00254759896953657,
3.32217611708959));
#7882=CARTESIAN_POINT('Ctrl Pts',(-2.94300132914192,0.00247067809074119,
3.17782388291039));
#7883=CARTESIAN_POINT('Ctrl Pts',(-2.93607565575577,-0.774344452547842,
3.21989646497146));
#7884=CARTESIAN_POINT('Ctrl Pts',(-2.61927127105561,-1.55615877069983,3.26196904703253));
#7885=CARTESIAN_POINT('Ctrl Pts',(-2.06758380697847,-2.0994678941542,3.30404162909359));
#7886=CARTESIAN_POINT('Ctrl Pts',(-1.37988398712591,-2.77672378748653,3.3564867343173));
#7887=CARTESIAN_POINT('Ctrl Pts',(-0.327208995338195,-3.08337625262348,
3.40893183954101));
#7888=CARTESIAN_POINT('Ctrl Pts',(0.616618861412321,-2.88139713307019,3.46137694476472));
#7889=CARTESIAN_POINT('Ctrl Pts',(1.56044671816283,-2.67941801351691,3.51382204998842));
#7890=CARTESIAN_POINT('Ctrl Pts',(2.39542743987614,-1.9688073092734,3.56626715521213));
#7891=CARTESIAN_POINT('Ctrl Pts',(2.74572565546219,-1.06941987852551,3.61871226043584));
#7892=CARTESIAN_POINT('Ctrl Pts',(3.09602387104824,-0.170032447777603,3.67115736565955));
#7893=CARTESIAN_POINT('Ctrl Pts',(2.96163958050702,0.918131709474696,3.72360247088326));
#7894=CARTESIAN_POINT('Ctrl Pts',(2.40306085127007,1.70527616384954,3.77604757610696));
#7895=CARTESIAN_POINT('Ctrl Pts',(1.84448212203313,2.49242061822439,3.82849268133067));
#7896=CARTESIAN_POINT('Ctrl Pts',(0.86170895410048,2.97854536972178,3.88093778655438));
#7897=CARTESIAN_POINT('Ctrl Pts',(-0.10290003671811,2.94483952623603,3.93338289177809));
#7898=CARTESIAN_POINT('Ctrl Pts',(-1.06750902753671,2.91113368275028,3.98582799700179));
#7899=CARTESIAN_POINT('Ctrl Pts',(-2.01395384124124,2.35759724428137,4.0382731022255));
#7900=CARTESIAN_POINT('Ctrl Pts',(-2.51622771244025,1.53338395412712,4.09071820744921));
#7901=CARTESIAN_POINT('Ctrl Pts',(-2.79430199366995,1.07707409733029,4.11975343260294));
#7902=CARTESIAN_POINT('Ctrl Pts',(-2.9362347477918,0.537799876108109,4.14878865775667));
#7903=CARTESIAN_POINT('Ctrl Pts',(-2.93758805006728,-0.000810565913221897,
4.1778238829104));
#7904=CARTESIAN_POINT('Origin',(0.,0.,0.));
#7905=CARTESIAN_POINT('',(-2.94644869531747,-0.000604754645607275,5.3221761170896));
#7906=CARTESIAN_POINT('',(-2.945679792052,-0.00146169071580815,5.1778238829104));
#7907=CARTESIAN_POINT('',(-2.942,-3.60291088309151E-16,0.));
#7908=CARTESIAN_POINT('Ctrl Pts',(-2.94644869531747,-0.000604754645607275,
5.3221761170896));
#7909=CARTESIAN_POINT('Ctrl Pts',(-2.94379550054715,0.929335583914262,5.27165540538226));
#7910=CARTESIAN_POINT('Ctrl Pts',(-2.46604729438678,1.86162808593007,5.22113469367492));
#7911=CARTESIAN_POINT('Ctrl Pts',(-1.70849336410036,2.40074283220066,5.17061398196758));
#7912=CARTESIAN_POINT('Ctrl Pts',(-0.923066988207087,2.95969305927406,5.11823447746308));
#7913=CARTESIAN_POINT('Ctrl Pts',(0.163133494924937,3.09600115191732,5.06585497295858));
#7914=CARTESIAN_POINT('Ctrl Pts',(1.06231690977038,2.74845383893534,5.01347546845407));
#7915=CARTESIAN_POINT('Ctrl Pts',(1.96150032461582,2.40090652595338,4.96109596394957));
#7916=CARTESIAN_POINT('Ctrl Pts',(2.67366667117468,1.56950380734618,4.90871645944506));
#7917=CARTESIAN_POINT('Ctrl Pts',(2.87899611438783,0.627612216959094,4.85633695494056));
#7918=CARTESIAN_POINT('Ctrl Pts',(3.08432555760098,-0.314279373428012,4.80395745043605));
#7919=CARTESIAN_POINT('Ctrl Pts',(2.7828180974684,-1.36665983559502,4.75157794593155));
#7920=CARTESIAN_POINT('Ctrl Pts',(2.10987477706647,-2.05692589721429,4.69919844142705));
#7921=CARTESIAN_POINT('Ctrl Pts',(1.43693145666455,-2.74719195883355,4.64681893692254));
#7922=CARTESIAN_POINT('Ctrl Pts',(0.392552275993288,-3.07534361990509,4.59443943241804));
#7923=CARTESIAN_POINT('Ctrl Pts',(-0.554252710038128,-2.89401445313919,
4.54205992791353));
#7924=CARTESIAN_POINT('Ctrl Pts',(-1.50105769606954,-2.71268528637328,4.48968042340903));
#7925=CARTESIAN_POINT('Ctrl Pts',(-2.35028848746111,-2.02187529176995,4.43730091890452));
#7926=CARTESIAN_POINT('Ctrl Pts',(-2.72057231514067,-1.13181358871689,4.38492141440002));
#7927=CARTESIAN_POINT('Ctrl Pts',(-2.86842638565151,-0.776412580180032,
4.36400631529654));
#7928=CARTESIAN_POINT('Ctrl Pts',(-2.93991718809614,-0.389242894153138,
4.34309121619307));
#7929=CARTESIAN_POINT('Ctrl Pts',(-2.93815144027097,-0.00144838940242836,
4.32217611708959));
#7930=CARTESIAN_POINT('Ctrl Pts',(-2.93758805006728,-0.000810565913221897,
4.1778238829104));
#7931=CARTESIAN_POINT('Ctrl Pts',(-2.93867916073716,-0.435069497448956,
4.20123376298038));
#7932=CARTESIAN_POINT('Ctrl Pts',(-2.84838634229403,-0.86889693810433,4.22464364305035));
#7933=CARTESIAN_POINT('Ctrl Pts',(-2.66438363654231,-1.25846258937073,4.24805352312033));
#7934=CARTESIAN_POINT('Ctrl Pts',(-2.25216276075188,-2.13120570087471,4.30049862834404));
#7935=CARTESIAN_POINT('Ctrl Pts',(-1.36961808047753,-2.78180178204309,4.35294373356775));
#7936=CARTESIAN_POINT('Ctrl Pts',(-0.413994103635433,-2.91740931891088,
4.40538883879146));
#7937=CARTESIAN_POINT('Ctrl Pts',(0.541629873206673,-3.05301685577867,4.45783394401517));
#7938=CARTESIAN_POINT('Ctrl Pts',(1.57033314661653,-2.67363584834587,4.51027904923887));
#7939=CARTESIAN_POINT('Ctrl Pts',(2.20908337968645,-1.9500304800975,4.56272415446258));
#7940=CARTESIAN_POINT('Ctrl Pts',(2.84783361275636,-1.22642511184914,4.61516925968629));
#7941=CARTESIAN_POINT('Ctrl Pts',(3.09663080548633,-0.158595382785209,4.66761436491));
#7942=CARTESIAN_POINT('Ctrl Pts',(2.84348819889812,0.772815058373636,4.7200594701337));
#7943=CARTESIAN_POINT('Ctrl Pts',(2.5903455923099,1.70422549953248,4.77250457535741));
#7944=CARTESIAN_POINT('Ctrl Pts',(1.83526318640351,2.49921665278624,4.82494968058112));
#7945=CARTESIAN_POINT('Ctrl Pts',(0.918113109485756,2.79995295852677,4.87739478580482));
#7946=CARTESIAN_POINT('Ctrl Pts',(0.000963032567994487,3.1006892642673,
4.92983989102853));
#7947=CARTESIAN_POINT('Ctrl Pts',(-1.07825471536113,2.90717072249458,4.98228499625224));
#7948=CARTESIAN_POINT('Ctrl Pts',(-1.83377059439506,2.30650247319915,5.03473010147595));
#7949=CARTESIAN_POINT('Ctrl Pts',(-2.5208993779335,1.76020496324304,5.08242802862077));
#7950=CARTESIAN_POINT('Ctrl Pts',(-2.94027519175655,0.877129838501974,5.13012595576559));
#7951=CARTESIAN_POINT('Ctrl Pts',(-2.945679792052,-0.00146169071580815,
5.1778238829104));
#7952=CARTESIAN_POINT('Origin',(0.,0.,0.));
#7953=CARTESIAN_POINT('',(-2.93949980478958,0.00219056232359141,6.3221761170896));
#7954=CARTESIAN_POINT('',(-2.94109090649655,0.00253660757586993,6.1778238829104));
#7955=CARTESIAN_POINT('',(-2.942,-3.60291088309151E-16,0.));
#7956=CARTESIAN_POINT('Ctrl Pts',(-2.93949980478958,0.00219056232359141,
6.3221761170896));
#7957=CARTESIAN_POINT('Ctrl Pts',(-2.94176361798241,0.320687415620876,6.30497860358046));
#7958=CARTESIAN_POINT('Ctrl Pts',(-2.89395610782771,0.638523376129415,6.28778109007132));
#7959=CARTESIAN_POINT('Ctrl Pts',(-2.79314214575126,0.938548174128603,6.27058357656218));
#7960=CARTESIAN_POINT('Ctrl Pts',(-2.48608697885785,1.85235180335153,6.21820407205768));
#7961=CARTESIAN_POINT('Ctrl Pts',(-1.68730919078036,2.60092740470414,6.16582456755317));
#7962=CARTESIAN_POINT('Ctrl Pts',(-0.75552410366601,2.84810446618733,6.11344506304867));
#7963=CARTESIAN_POINT('Ctrl Pts',(0.176260983448343,3.09528152767051,6.06106555854416));
#7964=CARTESIAN_POINT('Ctrl Pts',(1.24105336959955,2.84106004928427,6.00868605403966));
#7965=CARTESIAN_POINT('Ctrl Pts',(1.96067583262663,2.19960587399116,5.95630654953515));
#7966=CARTESIAN_POINT('Ctrl Pts',(2.68029829565369,1.55815169869806,5.90392704503064));
#7967=CARTESIAN_POINT('Ctrl Pts',(3.05475083555665,0.52946482649812,5.85154754052614));
#7968=CARTESIAN_POINT('Ctrl Pts',(2.91587421520356,-0.424491793382225,5.79916803602164));
#7969=CARTESIAN_POINT('Ctrl Pts',(2.77699759485047,-1.37844841326258,5.74678853151713));
#7970=CARTESIAN_POINT('Ctrl Pts',(2.12479181424134,-2.25767478082334,5.69440902701263));
#7971=CARTESIAN_POINT('Ctrl Pts',(1.25214960298458,-2.66732770639159,5.64202952250812));
#7972=CARTESIAN_POINT('Ctrl Pts',(0.379507391727844,-3.07698063195983,5.58965001800362));
#7973=CARTESIAN_POINT('Ctrl Pts',(-0.713571250176501,-3.01706011553558,
5.53727051349912));
#7974=CARTESIAN_POINT('Ctrl Pts',(-1.53620630199898,-2.5144752771182,5.48489100899462));
#7975=CARTESIAN_POINT('Ctrl Pts',(-2.35884135382146,-2.01189043870081,5.43251150449011));
#7976=CARTESIAN_POINT('Ctrl Pts',(-2.91103281556208,-1.0666412782903,5.3801319999856));
#7977=CARTESIAN_POINT('Ctrl Pts',(-2.94480241210512,-0.103220517333276,
5.3277524954811));
#7978=CARTESIAN_POINT('Ctrl Pts',(-2.94600079462919,-0.069031580495304,
5.32589370268393));
#7979=CARTESIAN_POINT('Ctrl Pts',(-2.94654631348559,-0.0348197596345374,
5.32403490988676));
#7980=CARTESIAN_POINT('Ctrl Pts',(-2.94644869531747,-0.000604754645607275,
5.3221761170896));
#7981=CARTESIAN_POINT('Ctrl Pts',(-2.945679792052,-0.00146169071580815,
5.1778238829104));
#7982=CARTESIAN_POINT('Ctrl Pts',(-2.94621768964176,-0.0889042840834332,
5.18257106098929));
#7983=CARTESIAN_POINT('Ctrl Pts',(-2.94265503660913,-0.176302465642187,
5.18731823906819));
#7984=CARTESIAN_POINT('Ctrl Pts',(-2.93484768462379,-0.263319805187537,
5.19206541714708));
#7985=CARTESIAN_POINT('Ctrl Pts',(-2.84859488567985,-1.22465587746066,5.24451052237078));
#7986=CARTESIAN_POINT('Ctrl Pts',(-2.24427527765324,-2.13951006518879,5.29695562759449));
#7987=CARTESIAN_POINT('Ctrl Pts',(-1.39390074925371,-2.59609494298297,5.34940073281819));
#7988=CARTESIAN_POINT('Ctrl Pts',(-0.543526220854162,-3.05267982077716,
5.4018458380419));
#7989=CARTESIAN_POINT('Ctrl Pts',(0.552903227918311,-3.05099538863739,5.45429094326562));
#7990=CARTESIAN_POINT('Ctrl Pts',(1.40187085321134,-2.59179983074767,5.50673604848932));
#7991=CARTESIAN_POINT('Ctrl Pts',(2.25083847850436,-2.13260427285796,5.55918115371303));
#7992=CARTESIAN_POINT('Ctrl Pts',(2.85234428031795,-1.21589758921833,5.61162625893673));
#7993=CARTESIAN_POINT('Ctrl Pts',(2.93564289965894,-0.254301037021637,5.66407136416044));
#7994=CARTESIAN_POINT('Ctrl Pts',(3.01894151899992,0.707295515175046,5.71651646938415));
#7995=CARTESIAN_POINT('Ctrl Pts',(2.5840329558683,1.71378193592877,5.76896157460786));
#7996=CARTESIAN_POINT('Ctrl Pts',(1.82667504784324,2.31212597436553,5.82140667983157));
#7997=CARTESIAN_POINT('Ctrl Pts',(1.06931713981816,2.9104700128023,5.87385178505528));
#7998=CARTESIAN_POINT('Ctrl Pts',(-0.010490113100349,3.1006716689221,5.92629689027898));
#7999=CARTESIAN_POINT('Ctrl Pts',(-0.92671182736886,2.79711877487579,5.97874199550269));
#8000=CARTESIAN_POINT('Ctrl Pts',(-1.84293354163737,2.49356588082949,6.0311871007264));
#8001=CARTESIAN_POINT('Ctrl Pts',(-2.59556971725588,1.69625843661705,6.08363220595011));
#8002=CARTESIAN_POINT('Ctrl Pts',(-2.84584930505901,0.764074593638618,6.13607731117382));
#8003=CARTESIAN_POINT('Ctrl Pts',(-2.91225724864025,0.516733559576513,6.14999283508601));
#8004=CARTESIAN_POINT('Ctrl Pts',(-2.94329794130529,0.259896865352817,6.16390835899821));
#8005=CARTESIAN_POINT('Ctrl Pts',(-2.94109090649655,0.00253660757586993,
6.1778238829104));
#8006=CARTESIAN_POINT('Origin',(0.,0.,0.));
#8007=CARTESIAN_POINT('',(-2.93998607517527,-0.0023358300504342,7.3221761170896));
#8008=CARTESIAN_POINT('',(-2.93846014819028,-0.00170708260597003,7.1778238829104));
#8009=CARTESIAN_POINT('',(-2.942,-3.60291088309151E-16,0.));
#8010=CARTESIAN_POINT('Ctrl Pts',(-2.93998607517527,-0.0023358300504342,
7.3221761170896));
#8011=CARTESIAN_POINT('Ctrl Pts',(-2.93483565594967,0.668801419715884,7.28592229727415));
#8012=CARTESIAN_POINT('Ctrl Pts',(-2.70624449366069,1.34311250814063,7.2496684774587));
#8013=CARTESIAN_POINT('Ctrl Pts',(-2.28495024526271,1.86051554631288,7.21341465764326));
#8014=CARTESIAN_POINT('Ctrl Pts',(-1.67626448210673,2.60805925085354,7.16103515313876));
#8015=CARTESIAN_POINT('Ctrl Pts',(-0.665321452888303,3.02806588999372,7.10865564863425));
#8016=CARTESIAN_POINT('Ctrl Pts',(0.293884302746592,2.93191878092119,7.05627614412975));
#8017=CARTESIAN_POINT('Ctrl Pts',(1.25309005838148,2.83577167184866,7.00389663962524));
#8018=CARTESIAN_POINT('Ctrl Pts',(2.16055854043283,2.22347081456344,6.95151713512074));
#8019=CARTESIAN_POINT('Ctrl Pts',(2.60876358347624,1.3699884259484,6.89913763061623));
#8020=CARTESIAN_POINT('Ctrl Pts',(3.05696862651966,0.516506037333356,6.84675812611173));
#8021=CARTESIAN_POINT('Ctrl Pts',(3.04591023055511,-0.578157882611513,6.79437862160723));
#8022=CARTESIAN_POINT('Ctrl Pts',(2.58055450279311,-1.42241139605186,6.74199911710272));
#8023=CARTESIAN_POINT('Ctrl Pts',(2.11519877503111,-2.26666490949219,6.68961961259822));
#8024=CARTESIAN_POINT('Ctrl Pts',(1.19554571547167,-2.86050801642801,6.63724010809371));
#8025=CARTESIAN_POINT('Ctrl Pts',(0.234593342362696,-2.93725751088208,6.5848606035892));
#8026=CARTESIAN_POINT('Ctrl Pts',(-0.726359030746288,-3.01400700533615,
6.5324810990847));
#8027=CARTESIAN_POINT('Ctrl Pts',(-1.72861071740481,-2.57366288730847,6.4801015945802));
#8028=CARTESIAN_POINT('Ctrl Pts',(-2.32207028787941,-1.813974999748,6.4277220900757));
#8029=CARTESIAN_POINT('Ctrl Pts',(-2.72068210106971,-1.30371182195979,6.39254009908033));
#8030=CARTESIAN_POINT('Ctrl Pts',(-2.93486858555413,-0.649377666932483,
6.35735810808496));
#8031=CARTESIAN_POINT('Ctrl Pts',(-2.93949980478958,0.00219056232359141,
6.3221761170896));
#8032=CARTESIAN_POINT('Ctrl Pts',(-2.94109090649655,0.00253660757586993,
6.1778238829104));
#8033=CARTESIAN_POINT('Ctrl Pts',(-2.9349800243151,-0.710047628629508,6.21635346422191));
#8034=CARTESIAN_POINT('Ctrl Pts',(-2.67397994955092,-1.42664569379386,6.25488304553342));
#8035=CARTESIAN_POINT('Ctrl Pts',(-2.20308134670334,-1.95680883878727,6.29341262684494));
#8036=CARTESIAN_POINT('Ctrl Pts',(-1.5621108005568,-2.67844818649031,6.34585773206864));
#8037=CARTESIAN_POINT('Ctrl Pts',(-0.532246708275948,-3.05466664015197,
6.39830283729235));
#8038=CARTESIAN_POINT('Ctrl Pts',(0.42295609402977,-2.91612352177857,6.45074794251606));
#8039=CARTESIAN_POINT('Ctrl Pts',(1.3781588963355,-2.77758040340517,6.50319304773977));
#8040=CARTESIAN_POINT('Ctrl Pts',(2.25870040866608,-2.12427571299673,6.55563815296348));
#8041=CARTESIAN_POINT('Ctrl Pts',(2.66823777423309,-1.25027014357196,6.60808325818718));
#8042=CARTESIAN_POINT('Ctrl Pts',(3.07777513980009,-0.376264574147203,6.66052836341089));
#8043=CARTESIAN_POINT('Ctrl Pts',(3.01630835860352,0.718441874293864,6.7129734686346));
#8044=CARTESIAN_POINT('Ctrl Pts',(2.51150440524776,1.54110800210975,6.76541857385831));
#8045=CARTESIAN_POINT('Ctrl Pts',(2.006700451892,2.36377412992563,6.81786367908202));
#8046=CARTESIAN_POINT('Ctrl Pts',(1.05855932637705,2.91439993711633,6.87030878430572));
#8047=CARTESIAN_POINT('Ctrl Pts',(0.0938513252260113,2.94514179293546,6.92275388952943));
#8048=CARTESIAN_POINT('Ctrl Pts',(-0.870856675925038,2.9758836487546,6.97519899475314));
#8049=CARTESIAN_POINT('Ctrl Pts',(-1.85213155271217,2.48674155320215,7.02764409997685));
#8050=CARTESIAN_POINT('Ctrl Pts',(-2.40828908863565,1.69788454181399,7.08008920520056));
#8051=CARTESIAN_POINT('Ctrl Pts',(-2.75376700818296,1.2078566962645,7.11266743110384));
#8052=CARTESIAN_POINT('Ctrl Pts',(-2.93520341737875,0.60217681128353,7.14524565700712));
#8053=CARTESIAN_POINT('Ctrl Pts',(-2.93846014819028,-0.00170708260597003,
7.1778238829104));
#8054=CARTESIAN_POINT('Origin',(0.,0.,0.));
#8055=CARTESIAN_POINT('',(-2.94622250669394,0.000937675328142526,8.3221761170896));
#8056=CARTESIAN_POINT('',(-2.94656696235233,-0.000396508504380587,8.1778238829104));
#8057=CARTESIAN_POINT('',(-2.942,-3.60291088309151E-16,0.));
#8058=CARTESIAN_POINT('Ctrl Pts',(-2.94622250669394,0.000937675328142526,
8.3221761170896));
#8059=CARTESIAN_POINT('Ctrl Pts',(-2.94645073222768,0.0548930361868928,
8.31924549547236));
#8060=CARTESIAN_POINT('Ctrl Pts',(-2.94509413407217,0.108836699779164,8.31631487385511));
#8061=CARTESIAN_POINT('Ctrl Pts',(-2.94211616003438,0.162690705921765,8.31338425223786));
#8062=CARTESIAN_POINT('Ctrl Pts',(-2.88889031756852,1.12523262560549,8.26100474773336));
#8063=CARTESIAN_POINT('Ctrl Pts',(-2.31771549444688,2.05913344782865,8.20862524322884));
#8064=CARTESIAN_POINT('Ctrl Pts',(-1.48509504480843,2.54499674522788,8.15624573872434));
#8065=CARTESIAN_POINT('Ctrl Pts',(-0.652474595169965,3.03086004262711,8.10386623421983));
#8066=CARTESIAN_POINT('Ctrl Pts',(0.44159148098532,3.06868581520241,8.05148672971533));
#8067=CARTESIAN_POINT('Ctrl Pts',(1.30577973958019,2.64148726651903,7.99910722521083));
#8068=CARTESIAN_POINT('Ctrl Pts',(2.16996799817506,2.21428871783565,7.94672772070633));
#8069=CARTESIAN_POINT('Ctrl Pts',(2.8042784392095,1.3220658478936,7.89434821620182));
#8070=CARTESIAN_POINT('Ctrl Pts',(2.92385476924452,0.36549831322338,7.84196871169732));
#8071=CARTESIAN_POINT('Ctrl Pts',(3.04343109927954,-0.591069221446826,7.78958920719281));
#8072=CARTESIAN_POINT('Ctrl Pts',(2.64827331831513,-1.61198142084519,7.73720970268831));
#8073=CARTESIAN_POINT('Ctrl Pts',(1.9158389819387,-2.23876678477201,7.68483019818381));
#8074=CARTESIAN_POINT('Ctrl Pts',(1.18340464556226,-2.86555214869884,7.6324506936793));
#8075=CARTESIAN_POINT('Ctrl Pts',(0.113693753773775,-3.09821067715411,7.58007118917479));
#8076=CARTESIAN_POINT('Ctrl Pts',(-0.812907669552306,-2.83226002346519,
7.52769168467029));
#8077=CARTESIAN_POINT('Ctrl Pts',(-1.73950909287838,-2.56630936977627,7.47531218016578));
#8078=CARTESIAN_POINT('Ctrl Pts',(-2.52300104774206,-1.80174953394315,7.42293267566128));
#8079=CARTESIAN_POINT('Ctrl Pts',(-2.81153277662714,-0.881929231056029,
7.37055317115678));
#8080=CARTESIAN_POINT('Ctrl Pts',(-2.90036087316611,-0.598751062127826,
7.35442748646772));
#8081=CARTESIAN_POINT('Ctrl Pts',(-2.94227697960606,-0.300857412821767,
7.33830180177866));
#8082=CARTESIAN_POINT('Ctrl Pts',(-2.93998607517527,-0.0023358300504342,
7.3221761170896));
#8083=CARTESIAN_POINT('Ctrl Pts',(-2.93846014819028,-0.00170708260597003,
7.1778238829104));
#8084=CARTESIAN_POINT('Ctrl Pts',(-2.94044617033292,-0.369968033311824,
7.19769076223082));
#8085=CARTESIAN_POINT('Ctrl Pts',(-2.87617048586605,-0.737561088352721,
7.21755764155125));
#8086=CARTESIAN_POINT('Ctrl Pts',(-2.7424268268773,-1.07785126568817,7.23742452087168));
#8087=CARTESIAN_POINT('Ctrl Pts',(-2.38936683413567,-1.97615813457835,7.28986962609539));
#8088=CARTESIAN_POINT('Ctrl Pts',(-1.55220665359259,-2.68419994513487,7.34231473131909));
#8089=CARTESIAN_POINT('Ctrl Pts',(-0.60776265660645,-2.88327813520494,7.3947598365428));
#8090=CARTESIAN_POINT('Ctrl Pts',(0.336681340379679,-3.082356325275,7.44720494176651));
#8091=CARTESIAN_POINT('Ctrl Pts',(1.38840915380886,-2.77247089485864,7.49965004699022));
#8092=CARTESIAN_POINT('Ctrl Pts',(2.07402481044015,-2.09310519028348,7.55209515221392));
#8093=CARTESIAN_POINT('Ctrl Pts',(2.75964046707144,-1.41373948570832,7.60454025743763));
#8094=CARTESIAN_POINT('Ctrl Pts',(3.07914396690482,-0.364893506974353,7.65698536266134));
#8095=CARTESIAN_POINT('Ctrl Pts',(2.8887227491853,0.5813339228528,7.70943046788505));
#8096=CARTESIAN_POINT('Ctrl Pts',(2.69830153146578,1.52756135267996,7.76187557310876));
#8097=CARTESIAN_POINT('Ctrl Pts',(1.99795559619334,2.37117023360031,7.81432067833246));
#8098=CARTESIAN_POINT('Ctrl Pts',(1.10291949457769,2.73244155291697,7.86676578355617));
#8099=CARTESIAN_POINT('Ctrl Pts',(0.207883392962048,3.09371287223363,7.91921088877988));
#8100=CARTESIAN_POINT('Ctrl Pts',(-0.881842874996807,2.97264662994661,7.97165599400359));
#8101=CARTESIAN_POINT('Ctrl Pts',(-1.67575975122609,2.42373627051487,8.0241010992273));
#8102=CARTESIAN_POINT('Ctrl Pts',(-2.45144772506959,1.88742928765845,8.07534202712166));
#8103=CARTESIAN_POINT('Ctrl Pts',(-2.94475435076587,0.942699847726619,8.12658295501603));
#8104=CARTESIAN_POINT('Ctrl Pts',(-2.94656696235233,-0.000396508504380587,
8.1778238829104));
#8105=CARTESIAN_POINT('Origin',(0.,0.,0.));
#8106=CARTESIAN_POINT('',(-2.93787859032851,0.00118007037484616,9.3221761170896));
#8107=CARTESIAN_POINT('',(-2.93938212312892,0.00216771032458683,9.1778238829104));
#8108=CARTESIAN_POINT('',(-2.942,-3.60291088309151E-16,0.));
#8109=CARTESIAN_POINT('Ctrl Pts',(-2.93787859032851,0.00118007037484616,
9.3221761170896));
#8110=CARTESIAN_POINT('Ctrl Pts',(-2.93938225399168,0.408942454113454,9.30018918916604));
#8111=CARTESIAN_POINT('Ctrl Pts',(-2.86009946358647,0.816145924853212,9.27820226124249));
#8112=CARTESIAN_POINT('Ctrl Pts',(-2.69715242952518,1.18654365111784,9.25621533331894));
#8113=CARTESIAN_POINT('Ctrl Pts',(-2.30896336853928,2.06894293121702,9.20383582881443));
#8114=CARTESIAN_POINT('Ctrl Pts',(-1.44594933104186,2.74245624053358,9.15145632430993));
#8115=CARTESIAN_POINT('Ctrl Pts',(-0.495674163844965,2.9046210644708,9.09907681980542));
#8116=CARTESIAN_POINT('Ctrl Pts',(0.454601003351916,3.06678588840801,9.04669731530092));
#8117=CARTESIAN_POINT('Ctrl Pts',(1.49213730024827,2.7176022269659,8.99431781079641));
#8118=CARTESIAN_POINT('Ctrl Pts',(2.15099835280526,2.01388208359571,8.94193830629191));
#8119=CARTESIAN_POINT('Ctrl Pts',(2.80985940536224,1.31016194022553,8.88955880178741));
#8120=CARTESIAN_POINT('Ctrl Pts',(3.09004521357986,0.251905314927287,8.8371792972829));
#8121=CARTESIAN_POINT('Ctrl Pts',(2.86572951288042,-0.685645923387644,8.7847997927784));
#8122=CARTESIAN_POINT('Ctrl Pts',(2.64141381218099,-1.62319716170258,8.73242028827389));
#8123=CARTESIAN_POINT('Ctrl Pts',(1.91259660256449,-2.44004301303419,8.68004078376939));
#8124=CARTESIAN_POINT('Ctrl Pts',(1.00657547791151,-2.76935400264746,8.62766127926488));
#8125=CARTESIAN_POINT('Ctrl Pts',(0.100554353258536,-3.09866499226073,8.57528177476038));
#8126=CARTESIAN_POINT('Ctrl Pts',(-0.982670686430926,-2.94044112015566,
8.52290227025587));
#8127=CARTESIAN_POINT('Ctrl Pts',(-1.75664477537062,-2.36573767553097,8.47052276575137));
#8128=CARTESIAN_POINT('Ctrl Pts',(-2.48731518632227,-1.82318876070292,8.42107388286411));
#8129=CARTESIAN_POINT('Ctrl Pts',(-2.94237161798714,-0.909460413780999,
8.37162499997686));
#8130=CARTESIAN_POINT('Ctrl Pts',(-2.94622250669394,0.000937675328142526,
8.3221761170896));
#8131=CARTESIAN_POINT('Ctrl Pts',(-2.94656696235233,-0.000396508504380587,
8.1778238829104));
#8132=CARTESIAN_POINT('Ctrl Pts',(-2.94660955927376,-0.0225595585939061,
8.17902806023974));
#8133=CARTESIAN_POINT('Ctrl Pts',(-2.94638072162746,-0.0447217067897041,
8.18023223756908));
#8134=CARTESIAN_POINT('Ctrl Pts',(-2.94587773547044,-0.0668776312364038,
8.18143641489842));
#8135=CARTESIAN_POINT('Ctrl Pts',(-2.92397135898579,-1.03182669697942,8.23388152012213));
#8136=CARTESIAN_POINT('Ctrl Pts',(-2.3820511215168,-1.98497035188899,8.28632662534583));
#8137=CARTESIAN_POINT('Ctrl Pts',(-1.5640421648278,-2.49728659914907,8.33877173056954));
#8138=CARTESIAN_POINT('Ctrl Pts',(-0.746033208138801,-3.00960284640916,
8.39121683579325));
#8139=CARTESIAN_POINT('Ctrl Pts',(0.348064467770205,-3.08109168601973,8.44366194101695));
#8140=CARTESIAN_POINT('Ctrl Pts',(1.22578367546087,-2.6795750856597,8.49610704624066));
#8141=CARTESIAN_POINT('Ctrl Pts',(2.10350288315153,-2.27805848529968,8.54855215146437));
#8142=CARTESIAN_POINT('Ctrl Pts',(2.76484362262384,-1.40353644496905,8.60099725668809));
#8143=CARTESIAN_POINT('Ctrl Pts',(2.91212808132915,-0.44964238612263,8.65344236191179));
#8144=CARTESIAN_POINT('Ctrl Pts',(3.05941254003446,0.504251672723784,8.7058874671355));
#8145=CARTESIAN_POINT('Ctrl Pts',(2.69264071797276,1.537517750086,8.75833257235921));
#8146=CARTESIAN_POINT('Ctrl Pts',(1.97690123029279,2.18506974304829,8.81077767758291));
#8147=CARTESIAN_POINT('Ctrl Pts',(1.26116174261282,2.83262173601059,8.86322278280662));
#8148=CARTESIAN_POINT('Ctrl Pts',(0.196454589314577,3.09445964457298,8.91566788803033));
#8149=CARTESIAN_POINT('Ctrl Pts',(-0.737982063629216,2.8527269003752,8.96811299325404));
#8150=CARTESIAN_POINT('Ctrl Pts',(-1.672418716573,2.61099415617743,9.02055809847774));
#8151=CARTESIAN_POINT('Ctrl Pts',(-2.47658486916233,1.86569075921951,9.07300320370145));
#8152=CARTESIAN_POINT('Ctrl Pts',(-2.78851523225651,0.952287217651892,9.12544830892515));
#8153=CARTESIAN_POINT('Ctrl Pts',(-2.89235416848512,0.648223031136026,9.1429068335869));
#8154=CARTESIAN_POINT('Ctrl Pts',(-2.94164516567622,0.325530543639097,9.16036535824865));
#8155=CARTESIAN_POINT('Ctrl Pts',(-2.93938212312892,0.00216771032458683,
9.1778238829104));
#8156=CARTESIAN_POINT('Origin',(0.,0.,0.));
#8157=CARTESIAN_POINT('',(-2.94242444587263,-0.00248500551853048,10.3221761170896));
#8158=CARTESIAN_POINT('',(-2.93989309841074,-0.00232834448912937,10.1778238829104));
#8159=CARTESIAN_POINT('',(-2.942,-3.60291088309151E-16,0.));
#8160=CARTESIAN_POINT('Ctrl Pts',(-2.94242444587263,-0.00248500551853048,
10.3221761170896));
#8161=CARTESIAN_POINT('Ctrl Pts',(-2.93565996783783,0.755676872330999,10.2811328828597));
#8162=CARTESIAN_POINT('Ctrl Pts',(-2.63573211439715,1.5185652175411,10.2400896486299));
#8163=CARTESIAN_POINT('Ctrl Pts',(-2.10792737213773,2.05892622612073,10.1990464144));
#8164=CARTESIAN_POINT('Ctrl Pts',(-1.43434130141424,2.74853664338077,10.1466669098955));
#8165=CARTESIAN_POINT('Ctrl Pts',(-0.389613404070186,3.07571802003838,10.094287405391));
#8166=CARTESIAN_POINT('Ctrl Pts',(0.557026464387836,2.89349108573471,10.0419079008865));
#8167=CARTESIAN_POINT('Ctrl Pts',(1.50366633284582,2.71126415143105,9.98952839638201));
#8168=CARTESIAN_POINT('Ctrl Pts',(2.35221817241779,2.01962890616612,9.9371488918775));
#8169=CARTESIAN_POINT('Ctrl Pts',(2.72164717416933,1.12921048240304,9.884769387373));
#8170=CARTESIAN_POINT('Ctrl Pts',(3.09107617592089,0.238792058639911,9.83238988286849));
#8171=CARTESIAN_POINT('Ctrl Pts',(2.981382339852,-0.85040954362138,9.78001037836398));
#8172=CARTESIAN_POINT('Ctrl Pts',(2.44180970997212,-1.64926869616342,9.72763087385948));
#8173=CARTESIAN_POINT('Ctrl Pts',(1.90223708009224,-2.44812784870545,9.67525136935497));
#8174=CARTESIAN_POINT('Ctrl Pts',(0.93278565640137,-2.95664455152821,9.62287186485046));
#8175=CARTESIAN_POINT('Ctrl Pts',(-0.031174037472469,-2.94644704900523,
9.57049236034596));
#8176=CARTESIAN_POINT('Ctrl Pts',(-0.995133731346301,-2.93624954648225,
9.51811285584146));
#8177=CARTESIAN_POINT('Ctrl Pts',(-1.9536016954031,-2.40733783861356,9.46573335133695));
#8178=CARTESIAN_POINT('Ctrl Pts',(-2.4761536351943,-1.5972393592383,9.41335384683245));
#8179=CARTESIAN_POINT('Ctrl Pts',(-2.77935810415337,-1.1271894741653,9.3829612702515));
#8180=CARTESIAN_POINT('Ctrl Pts',(-2.93580007289335,-0.56247072784923,9.35256869367055));
#8181=CARTESIAN_POINT('Ctrl Pts',(-2.93787859032851,0.00118007037484616,
9.3221761170896));
#8182=CARTESIAN_POINT('Ctrl Pts',(-2.93938212312892,0.00216771032458683,
9.1778238829104));
#8183=CARTESIAN_POINT('Ctrl Pts',(-2.93484702512206,-0.645845798130107,
9.21281046347236));
#8184=CARTESIAN_POINT('Ctrl Pts',(-2.72327366311651,-1.29655137950586,9.24779704403432));
#8185=CARTESIAN_POINT('Ctrl Pts',(-2.32875660055073,-1.80542543875765,9.28278362459629));
#8186=CARTESIAN_POINT('Ctrl Pts',(-1.73737303215174,-2.56823086742229,9.33522872981999));
#8187=CARTESIAN_POINT('Ctrl Pts',(-0.73491132175476,-3.01233803857425,9.3876738350437));
#8188=CARTESIAN_POINT('Ctrl Pts',(0.227407657021308,-2.93784857599215,9.44011894026741));
#8189=CARTESIAN_POINT('Ctrl Pts',(1.1897266357974,-2.86335911341005,9.49256404549111));
#8190=CARTESIAN_POINT('Ctrl Pts',(2.11190288295256,-2.27027301709385,9.54500915071482));
#8191=CARTESIAN_POINT('Ctrl Pts',(2.57885359588429,-1.42554607687093,9.59745425593853));
#8192=CARTESIAN_POINT('Ctrl Pts',(3.045804308816,-0.580819136648041,9.64989936116224));
#8193=CARTESIAN_POINT('Ctrl Pts',(3.05752948752431,0.515548647481566,9.70234446638595));
#8194=CARTESIAN_POINT('Ctrl Pts',(2.60875076544854,1.37006875926759,9.75478957160966));
#8195=CARTESIAN_POINT('Ctrl Pts',(2.15997204337277,2.22458887105361,9.80723467683336));
#8196=CARTESIAN_POINT('Ctrl Pts',(1.25068942051291,2.83726131049606,9.85967978205706));
#8197=CARTESIAN_POINT('Ctrl Pts',(0.290183858659324,2.93231357229399,9.91212488728077));
#8198=CARTESIAN_POINT('Ctrl Pts',(-0.67032170319427,3.02736583409193,9.96456999250448));
#8199=CARTESIAN_POINT('Ctrl Pts',(-1.68205020404159,2.60479791824536,10.0170150977282));
#8200=CARTESIAN_POINT('Ctrl Pts',(-2.28961248249041,1.85481470515708,10.0694602029519));
#8201=CARTESIAN_POINT('Ctrl Pts',(-2.708067067946,1.33826862311137,10.1055814296047));
#8202=CARTESIAN_POINT('Ctrl Pts',(-2.93479827488144,0.666407318052135,10.1417026562576));
#8203=CARTESIAN_POINT('Ctrl Pts',(-2.93989309841074,-0.00232834448912937,
10.1778238829104));
#8204=CARTESIAN_POINT('Origin',(0.,0.,-1.84858989190501));
#8205=CARTESIAN_POINT('',(-2.3720921752204,-0.00200333509135781,10.651410108095));
#8206=CARTESIAN_POINT('',(-2.37533330856671,0.000645282184899808,10.848589891905));
#8207=CARTESIAN_POINT('',(-2.37175,-1.78696459712734E-13,-1.84858989190501));
#8208=CARTESIAN_POINT('',(-2.34668236863852,0.343918483395543,11.62825));
#8209=CARTESIAN_POINT('Ctrl Pts',(-2.3720921752204,-0.00200333509135741,
10.651410108095));
#8210=CARTESIAN_POINT('Ctrl Pts',(-2.37359839777753,-0.170820576644891,
10.6627463783696));
#8211=CARTESIAN_POINT('Ctrl Pts',(-2.28072670946568,-1.11802807678178,10.7264621531488));
#8212=CARTESIAN_POINT('Ctrl Pts',(-1.0098707589218,-2.60498459805753,10.8425574324324));
#8213=CARTESIAN_POINT('Ctrl Pts',(1.61803174729613,-2.2773674076414,10.999695945946));
#8214=CARTESIAN_POINT('Ctrl Pts',(2.79127527466209,0.0946110570183949,11.1568344594594));
#8215=CARTESIAN_POINT('Ctrl Pts',(1.46022534703361,2.38369320998594,11.313972972973));
#8216=CARTESIAN_POINT('Ctrl Pts',(-1.1878082887304,2.52773050943662,11.4711114864865));
#8217=CARTESIAN_POINT('Ctrl Pts',(-2.23349531079268,1.11623543008163,11.5758704954955));
#8218=CARTESIAN_POINT('Ctrl Pts',(-2.34668236863853,0.343918483395475,11.62825));
#8219=CARTESIAN_POINT('',(-0.439445221994028,2.33068358199191,11.62825));
#8220=CARTESIAN_POINT('Origin',(0.,0.,11.62825));
#8221=CARTESIAN_POINT('Ctrl Pts',(-2.37533330856671,0.000645282184899929,
10.848589891905));
#8222=CARTESIAN_POINT('Ctrl Pts',(-2.37266626526946,-0.74297942345447,10.8986961737085));
#8223=CARTESIAN_POINT('Ctrl Pts',(-1.5987407489101,-2.26979394046941,11.0012475607357));
#8224=CARTESIAN_POINT('Ctrl Pts',(0.989622905930635,-2.61290295808564,11.1562440529866));
#8225=CARTESIAN_POINT('Ctrl Pts',(2.72902843688469,-0.61088887604173,11.3135793686578));
#8226=CARTESIAN_POINT('Ctrl Pts',(2.00599839187704,1.9449087769569,11.4709146843289));
#8227=CARTESIAN_POINT('Ctrl Pts',(0.328567026486064,2.47549058867235,11.5758048947763));
#8228=CARTESIAN_POINT('Ctrl Pts',(-0.439445221994061,2.3306835819919,11.62825));
#8229=CARTESIAN_POINT('Origin',(0.,0.,-1.84858989190501));
#8230=CARTESIAN_POINT('',(-2.36842744616303,0.000951336475574988,9.65141010809499));
#8231=CARTESIAN_POINT('',(-2.37005148067835,-0.00187703978340947,9.84858989190503));
#8232=CARTESIAN_POINT('',(-2.37175,-1.78696459712734E-13,-1.84858989190501));
#8233=CARTESIAN_POINT('Ctrl Pts',(-2.36842744616303,0.000951336475575049,
9.65141010809499));
#8234=CARTESIAN_POINT('Ctrl Pts',(-2.36675180927421,-0.453446617531184,
9.68180268467594));
#8235=CARTESIAN_POINT('Ctrl Pts',(-2.02327622703562,-1.69331275929724,9.76457476576139));
#8236=CARTESIAN_POINT('Ctrl Pts',(-0.0295588149451427,-2.79350652787453,
9.89972635135136));
#8237=CARTESIAN_POINT('Ctrl Pts',(2.31506703223917,-1.56365490661018,10.0568648648649));
#8238=CARTESIAN_POINT('Ctrl Pts',(2.58036243233743,1.07058768363104,10.2140033783784));
#8239=CARTESIAN_POINT('Ctrl Pts',(0.528133174514654,2.74331293137788,10.3711418918919));
#8240=CARTESIAN_POINT('Ctrl Pts',(-1.81626974066498,2.00910742659655,10.5169441351307));
#8241=CARTESIAN_POINT('Ctrl Pts',(-2.36663886088356,0.609203474490441,10.6103668738651));
#8242=CARTESIAN_POINT('Ctrl Pts',(-2.3720921752204,-0.00200333509135741,
10.651410108095));
#8243=CARTESIAN_POINT('Ctrl Pts',(-2.37005148067835,-0.0018770397834093,
9.84858989190503));
#8244=CARTESIAN_POINT('Ctrl Pts',(-2.37190764427919,-0.245513112411714,
9.8649137704759));
#8245=CARTESIAN_POINT('Ctrl Pts',(-2.22599738542921,-1.26973141402768,9.93368275427047));
#8246=CARTESIAN_POINT('Ctrl Pts',(-0.757654725048104,-2.69016151139635,
10.0548968432888));
#8247=CARTESIAN_POINT('Ctrl Pts',(1.83027666927001,-2.11210170665972,10.2122321589599));
#8248=CARTESIAN_POINT('Ctrl Pts',(2.77060484795253,0.367287133540841,10.369567474631));
#8249=CARTESIAN_POINT('Ctrl Pts',(1.21665350181368,2.51610800548609,10.5269027903021));
#8250=CARTESIAN_POINT('Ctrl Pts',(-1.43234772356642,2.39972494583597,10.6842381059733));
#8251=CARTESIAN_POINT('Ctrl Pts',(-2.35921176770024,0.848280000432971,10.7914671398409));
#8252=CARTESIAN_POINT('Ctrl Pts',(-2.37545779881228,0.0353556381482985,
10.8462510684848));
#8253=CARTESIAN_POINT('Ctrl Pts',(-2.37533330856671,0.000645282184899929,
10.848589891905));
#8254=CARTESIAN_POINT('Origin',(0.,0.,-1.84858989190501));
#8255=CARTESIAN_POINT('',(-2.37515405515002,0.000755925037124906,8.65141010809499));
#8256=CARTESIAN_POINT('',(-2.36963954810708,0.00174754145538428,8.84858989190503));
#8257=CARTESIAN_POINT('',(-2.37175,-1.78696459712734E-13,-1.84858989190501));
#8258=CARTESIAN_POINT('Ctrl Pts',(-2.37515405515002,0.00075592503712492,
8.65141010809499));
#8259=CARTESIAN_POINT('Ctrl Pts',(-2.37204958700235,-0.733179040239741,
8.70085899098224));
#8260=CARTESIAN_POINT('Ctrl Pts',(-1.61660279875904,-2.25007474146859,8.80268737837401));
#8261=CARTESIAN_POINT('Ctrl Pts',(0.954326572136137,-2.62560372673677,8.95689527027026));
#8262=CARTESIAN_POINT('Ctrl Pts',(2.71697669134881,-0.650055649344734,9.11403378378378));
#8263=CARTESIAN_POINT('Ctrl Pts',(2.03934512373477,1.90934627218937,9.2711722972973));
#8264=CARTESIAN_POINT('Ctrl Pts',(-0.469944521571767,2.75384968723896,9.42831081081079));
#8265=CARTESIAN_POINT('Ctrl Pts',(-2.15345863304216,1.44000181080629,9.55505674774338));
#8266=CARTESIAN_POINT('Ctrl Pts',(-2.36963965360463,0.329676840769313,9.62942318017144));
#8267=CARTESIAN_POINT('Ctrl Pts',(-2.36842744616303,0.000951336475575049,
9.65141010809499));
#8268=CARTESIAN_POINT('Ctrl Pts',(-2.36963954810708,0.00174754145538407,
8.84858989190503));
#8269=CARTESIAN_POINT('Ctrl Pts',(-2.36598349144566,-0.520661037292834,
8.88357647246699));
#8270=CARTESIAN_POINT('Ctrl Pts',(-1.9397431197991,-1.83158688452099,8.97100815825266));
#8271=CARTESIAN_POINT('Ctrl Pts',(0.215690902196592,-2.78647992051942,9.11088494926201));
#8272=CARTESIAN_POINT('Ctrl Pts',(2.4459813653409,-1.35209655994371,9.26822026493315));
#8273=CARTESIAN_POINT('Ctrl Pts',(2.47433880171217,1.29947749716991,9.42555558060427));
#8274=CARTESIAN_POINT('Ctrl Pts',(0.275231669725872,2.78123058171878,9.58289089627539));
#8275=CARTESIAN_POINT('Ctrl Pts',(-1.91777323438188,1.86527979947427,9.72390233337565));
#8276=CARTESIAN_POINT('Ctrl Pts',(-2.36594419049973,0.537237102851684,9.81246866525219));
#8277=CARTESIAN_POINT('Ctrl Pts',(-2.37005148067835,-0.0018770397834093,
9.84858989190503));
#8278=CARTESIAN_POINT('Origin',(0.,0.,-1.84858989190501));
#8279=CARTESIAN_POINT('',(-2.37012643568897,-0.00188307441280249,7.65141010809499));
#8280=CARTESIAN_POINT('',(-2.37543174471759,-0.000319652972777529,7.84858989190503));
#8281=CARTESIAN_POINT('',(-2.37175,-1.78696459712734E-13,-1.84858989190501));
#8282=CARTESIAN_POINT('Ctrl Pts',(-2.37012643568897,-0.00188307441280247,
7.65141010809499));
#8283=CARTESIAN_POINT('Ctrl Pts',(-2.37197329244753,-0.242542001652036,
7.66753579278404));
#8284=CARTESIAN_POINT('Ctrl Pts',(-2.22842022339473,-1.26275955622086,7.7360409819776));
#8285=CARTESIAN_POINT('Ctrl Pts',(-0.770711640749916,-2.68524440462409,
7.85692567567567));
#8286=CARTESIAN_POINT('Ctrl Pts',(1.81639251383808,-2.12255793467458,8.01406418918919));
#8287=CARTESIAN_POINT('Ctrl Pts',(2.77208469636934,0.346526200869026,8.1712027027027));
#8288=CARTESIAN_POINT('Ctrl Pts',(1.23799993580832,2.50437418705365,8.32834121621622));
#8289=CARTESIAN_POINT('Ctrl Pts',(-1.40800742257503,2.4128922603655,8.48547972972973));
#8290=CARTESIAN_POINT('Ctrl Pts',(-2.35469744140074,0.865004378788607,8.59316936035599));
#8291=CARTESIAN_POINT('Ctrl Pts',(-2.37533804356255,0.0442530790537146,
8.64847948647774));
#8292=CARTESIAN_POINT('Ctrl Pts',(-2.37515405515002,0.00075592503712492,
8.65141010809499));
#8293=CARTESIAN_POINT('Ctrl Pts',(-2.37543174471759,-0.000319652972777509,
7.84858989190503));
#8294=CARTESIAN_POINT('Ctrl Pts',(-2.37546608504675,-0.0181868229420618,
7.84979406923436));
#8295=CARTESIAN_POINT('Ctrl Pts',(-2.36724692977477,-0.814184073087101,
7.9034433517874));
#8296=CARTESIAN_POINT('Ctrl Pts',(-1.48345697628832,-2.36861723168749,8.00953773956416));
#8297=CARTESIAN_POINT('Ctrl Pts',(1.16262680634646,-2.54151354917186,8.16687305523529));
#8298=CARTESIAN_POINT('Ctrl Pts',(2.76208455499713,-0.426475157784177,8.3242083709064));
#8299=CARTESIAN_POINT('Ctrl Pts',(1.8750440359881,2.07248692819523,8.48154368657753));
#8300=CARTESIAN_POINT('Ctrl Pts',(-0.699958537943023,2.7057439570526,8.63887900224866));
#8301=CARTESIAN_POINT('Ctrl Pts',(-2.21235813584821,1.30404785948979,8.76122773735781));
#8302=CARTESIAN_POINT('Ctrl Pts',(-2.37146394347132,0.262432721575661,8.83113136724327));
#8303=CARTESIAN_POINT('Ctrl Pts',(-2.36963954810708,0.00174754145538407,
8.84858989190503));
#8304=CARTESIAN_POINT('Origin',(0.,0.,-1.84858989190501));
#8305=CARTESIAN_POINT('',(-2.36973441944585,0.0017659640348839,6.65141010809499));
#8306=CARTESIAN_POINT('',(-2.36889628024144,-0.00137619754296547,6.84858989190503));
#8307=CARTESIAN_POINT('',(-2.37175,-1.78696459712734E-13,-1.84858989190501));
#8308=CARTESIAN_POINT('Ctrl Pts',(-2.36973441944585,0.00176596403488379,
6.65141010809499));
#8309=CARTESIAN_POINT('Ctrl Pts',(-2.36600087280351,-0.523508321396127,
6.68659209909035));
#8310=CARTESIAN_POINT('Ctrl Pts',(-1.93625564677593,-1.83636884117464,6.77415359459022));
#8311=CARTESIAN_POINT('Ctrl Pts',(0.222416181733502,-2.78479173243988,6.91409459459459));
#8312=CARTESIAN_POINT('Ctrl Pts',(2.4466042959518,-1.34857753576241,7.0712331081081));
#8313=CARTESIAN_POINT('Ctrl Pts',(2.47334911304448,1.29887571249989,7.22837162162162));
#8314=CARTESIAN_POINT('Ctrl Pts',(0.278629494786153,2.77973012269657,7.38551013513513));
#8315=CARTESIAN_POINT('Ctrl Pts',(-1.91543890246215,1.86818192765693,7.52652296395959));
#8316=CARTESIAN_POINT('Ctrl Pts',(-2.36597432596829,0.539167154048567,7.61515628827954));
#8317=CARTESIAN_POINT('Ctrl Pts',(-2.37012643568897,-0.00188307441280247,
7.65141010809499));
#8318=CARTESIAN_POINT('Ctrl Pts',(-2.36889628024144,-0.0013761975429653,
6.84858989190503));
#8319=CARTESIAN_POINT('Ctrl Pts',(-2.37049735026751,-0.298256860301772,
6.86845677122545));
#8320=CARTESIAN_POINT('Ctrl Pts',(-2.18189218700624,-1.37689100842058,6.94076875576958));
#8321=CARTESIAN_POINT('Ctrl Pts',(-0.57644849505612,-2.73472106868152,7.06552584553741));
#8322=CARTESIAN_POINT('Ctrl Pts',(1.96716344393165,-1.98526073259378,7.22286116120855));
#8323=CARTESIAN_POINT('Ctrl Pts',(2.73988515609665,0.551381466653972,7.38019647687966));
#8324=CARTESIAN_POINT('Ctrl Pts',(1.04609303646807,2.5916561403346,7.53753179255079));
#8325=CARTESIAN_POINT('Ctrl Pts',(-1.56924738212969,2.3010974504224,7.69366293089257));
#8326=CARTESIAN_POINT('Ctrl Pts',(-2.3739704729535,0.759975650525201,7.79734896401065));
#8327=CARTESIAN_POINT('Ctrl Pts',(-2.37543174471759,-0.000319652972777509,
7.84858989190503));
#8328=CARTESIAN_POINT('Origin',(0.,0.,-1.84858989190501));
#8329=CARTESIAN_POINT('',(-2.37533640146812,-0.000487534612837604,5.65141010809499));
#8330=CARTESIAN_POINT('',(-2.3710171167516,0.00204493508413422,5.84858989190502));
#8331=CARTESIAN_POINT('',(-2.37175,-1.78696459712734E-13,-1.84858989190501));
#8332=CARTESIAN_POINT('Ctrl Pts',(-2.37533640146812,-0.000487534612837498,
5.65141010809499));
#8333=CARTESIAN_POINT('Ctrl Pts',(-2.3754150982357,-0.0280706202968775,
5.65326890089215));
#8334=CARTESIAN_POINT('Ctrl Pts',(-2.36258260410634,-0.832851216236821,
5.70750719819383));
#8335=CARTESIAN_POINT('Ctrl Pts',(-1.45646562934828,-2.38395507960311,5.81412499999999));
#8336=CARTESIAN_POINT('Ctrl Pts',(1.18715361157964,-2.5288733170224,5.97126351351352));
#8337=CARTESIAN_POINT('Ctrl Pts',(2.76451839080433,-0.402457473451116,6.12840202702702));
#8338=CARTESIAN_POINT('Ctrl Pts',(1.8589019956498,2.08542976904401,6.28554054054054));
#8339=CARTESIAN_POINT('Ctrl Pts',(-0.716306714602523,2.70026640197657,6.44267905405405));
#8340=CARTESIAN_POINT('Ctrl Pts',(-2.21563200675447,1.29517183256302,6.5646355765722));
#8341=CARTESIAN_POINT('Ctrl Pts',(-2.37155943608083,0.258528340584143,6.63421259458585));
#8342=CARTESIAN_POINT('Ctrl Pts',(-2.36973441944585,0.00176596403488379,
6.65141010809499));
#8343=CARTESIAN_POINT('Ctrl Pts',(-2.3710171167516,0.00204493508413416,
5.84858989190502));
#8344=CARTESIAN_POINT('Ctrl Pts',(-2.36609071130836,-0.572418580286349,
5.88711947321653));
#8345=CARTESIAN_POINT('Ctrl Pts',(-1.86927748327345,-1.93646185988882,5.97809415975175));
#8346=CARTESIAN_POINT('Ctrl Pts',(0.401163844498212,-2.76587414046649,6.12151395151068));
#8347=CARTESIAN_POINT('Ctrl Pts',(2.53076037597685,-1.18585163930103,6.2788492671818));
#8348=CARTESIAN_POINT('Ctrl Pts',(2.38210248511723,1.46170446446183,6.43618458285292));
#8349=CARTESIAN_POINT('Ctrl Pts',(0.0890157606711408,2.793397283841,6.59351989852405));
#8350=CARTESIAN_POINT('Ctrl Pts',(-1.98453634187054,1.75978107224967,6.73098833487474));
#8351=CARTESIAN_POINT('Ctrl Pts',(-2.36627080393209,0.485456441931073,6.81601166600174));
#8352=CARTESIAN_POINT('Ctrl Pts',(-2.36889628024144,-0.0013761975429653,
6.84858989190503));
#8353=CARTESIAN_POINT('Origin',(0.,0.,-1.84858989190501));
#8354=CARTESIAN_POINT('',(-2.36864740940268,-0.0011676470311218,4.65141010809498));
#8355=CARTESIAN_POINT('',(-2.37471653528189,-0.00117837014130401,4.84858989190502));
#8356=CARTESIAN_POINT('',(-2.37175,-1.78696459712734E-13,-1.84858989190501));
#8357=CARTESIAN_POINT('Ctrl Pts',(-2.36864740940268,-0.00116764703112199,
4.65141010809498));
#8358=CARTESIAN_POINT('Ctrl Pts',(-2.37007090104248,-0.313795660845675,
4.67232520719846));
#8359=CARTESIAN_POINT('Ctrl Pts',(-2.16810014725707,-1.40760004764448,4.74561981080643));
#8360=CARTESIAN_POINT('Ctrl Pts',(-0.525482821607704,-2.74379331497496,
4.87129391891892));
#8361=CARTESIAN_POINT('Ctrl Pts',(2.00035639160479,-1.95015595724574,5.02843243243243));
#8362=CARTESIAN_POINT('Ctrl Pts',(2.72955454106374,0.595034417816705,5.18557094594594));
#8363=CARTESIAN_POINT('Ctrl Pts',(1.0071746643292,2.60578839251754,5.34270945945947));
#8364=CARTESIAN_POINT('Ctrl Pts',(-1.58873507575841,2.28002578161798,5.49798918017579));
#8365=CARTESIAN_POINT('Ctrl Pts',(-2.37319747737008,0.7492017916888,5.60088939638765));
#8366=CARTESIAN_POINT('Ctrl Pts',(-2.37533640146812,-0.000487534612837498,
5.65141010809499));
#8367=CARTESIAN_POINT('Ctrl Pts',(-2.37471653528189,-0.00117837014130423,
4.84858989190502));
#8368=CARTESIAN_POINT('Ctrl Pts',(-2.37515017179056,-0.0716719020310164,
4.85333706998391));
#8369=CARTESIAN_POINT('Ctrl Pts',(-2.34054813360425,-0.920521113001663,
4.91052935328651));
#8370=CARTESIAN_POINT('Ctrl Pts',(-1.32208186928512,-2.46233460804071,5.02016674181281));
#8371=CARTESIAN_POINT('Ctrl Pts',(1.32964132424929,-2.45826079574207,5.17750205748394));
#8372=CARTESIAN_POINT('Ctrl Pts',(2.78438780839412,-0.241198514719961,5.33483737315506));
#8373=CARTESIAN_POINT('Ctrl Pts',(1.73255804842731,2.19299676239354,5.49217268882618));
#8374=CARTESIAN_POINT('Ctrl Pts',(-0.878964234485193,2.65300095467984,5.64950800449731));
#8375=CARTESIAN_POINT('Ctrl Pts',(-2.25346115704322,1.19692341827648,5.76831373885692));
#8376=CARTESIAN_POINT('Ctrl Pts',(-2.37279636039799,0.20952086689332,5.83467436799283));
#8377=CARTESIAN_POINT('Ctrl Pts',(-2.3710171167516,0.00204493508413416,
5.84858989190502));
#8378=CARTESIAN_POINT('Origin',(0.,0.,-1.84858989190501));
#8379=CARTESIAN_POINT('',(-2.37165914320747,0.00205379600805495,3.65141010809498));
#8380=CARTESIAN_POINT('',(-2.36819322153198,-0.000653453332863235,3.84858989190502));
#8381=CARTESIAN_POINT('',(-2.37175,-1.78696459712734E-13,-1.84858989190501));
#8382=CARTESIAN_POINT('Ctrl Pts',(-2.37165914320747,0.0020537960080548,
3.65141010809498));
#8383=CARTESIAN_POINT('Ctrl Pts',(-2.36638740749304,-0.593495286532831,
3.69138151350476));
#8384=CARTESIAN_POINT('Ctrl Pts',(-1.83931642681201,-1.97778866762885,3.78373242341905));
#8385=CARTESIAN_POINT('Ctrl Pts',(0.47257542983782,-2.75339906613161,3.92846283783783));
#8386=CARTESIAN_POINT('Ctrl Pts',(2.55822296043148,-1.12251023841371,4.08560135135135));
#8387=CARTESIAN_POINT('Ctrl Pts',(2.34617571991457,1.51657292659299,4.24273986486486));
#8388=CARTESIAN_POINT('Ctrl Pts',(0.0268861606557786,2.79353021925399,4.39987837837838));
#8389=CARTESIAN_POINT('Ctrl Pts',(-2.00464048744226,1.72543877128143,4.53610179278842));
#8390=CARTESIAN_POINT('Ctrl Pts',(-2.36650592693501,0.469145905762286,4.61994570269395));
#8391=CARTESIAN_POINT('Ctrl Pts',(-2.36864740940268,-0.00116764703112199,
4.65141010809498));
#8392=CARTESIAN_POINT('Ctrl Pts',(-2.36819322153198,-0.000653453332863235,
3.84858989190502));
#8393=CARTESIAN_POINT('Ctrl Pts',(-2.36907284142701,-0.350739660290616,
3.871999771975));
#8394=CARTESIAN_POINT('Ctrl Pts',(-2.13320735842129,-1.48399610964751,3.94785475726868));
#8395=CARTESIAN_POINT('Ctrl Pts',(-0.392663608746353,-2.76709368867159,
4.07615484778607));
#8396=CARTESIAN_POINT('Ctrl Pts',(2.09526330020315,-1.8495577562663,4.23349016345719));
#8397=CARTESIAN_POINT('Ctrl Pts',(2.69698125586998,0.732996791565816,4.39082547912832));
#8398=CARTESIAN_POINT('Ctrl Pts',(0.870808554093777,2.65568911080063,4.54816079479944));
#8399=CARTESIAN_POINT('Ctrl Pts',(-1.66053522846232,2.20178445767042,4.70074893239168));
#8400=CARTESIAN_POINT('Ctrl Pts',(-2.37035951259304,0.707115123883991,4.8008919647602));
#8401=CARTESIAN_POINT('Ctrl Pts',(-2.37471653528189,-0.00117837014130423,
4.84858989190502));
#8402=CARTESIAN_POINT('Origin',(0.,0.,-1.84858989190501));
#8403=CARTESIAN_POINT('',(-2.37406517885066,-0.00153607482357252,2.65141010809498));
#8404=CARTESIAN_POINT('',(-2.37255724078598,0.00199178475905649,2.84858989190502));
#8405=CARTESIAN_POINT('',(-2.37175,-1.78696459712734E-13,-1.84858989190501));
#8406=CARTESIAN_POINT('Ctrl Pts',(-2.37406517885066,-0.00153607482357281,
2.65141010809498));
#8407=CARTESIAN_POINT('Ctrl Pts',(-2.37481281249436,-0.100330398866114,
2.65805831530656));
#8408=CARTESIAN_POINT('Ctrl Pts',(-2.32469515905834,-0.976735840432517,
2.71708602702265));
#8409=CARTESIAN_POINT('Ctrl Pts',(-1.23560715428754,-2.50555554774625,2.82849324324324));
#8410=CARTESIAN_POINT('Ctrl Pts',(1.41031161531747,-2.41154623133624,2.98563175675675));
#8411=CARTESIAN_POINT('Ctrl Pts',(2.78954424185296,-0.151581281506301,3.14277027027027));
#8412=CARTESIAN_POINT('Ctrl Pts',(1.66331845351111,2.24452793077997,3.29990878378378));
#8413=CARTESIAN_POINT('Ctrl Pts',(-0.956834235921451,2.62469088021855,3.45704729729729));
#8414=CARTESIAN_POINT('Ctrl Pts',(-2.26971028444252,1.15040938517441,3.57421440540103));
#8415=CARTESIAN_POINT('Ctrl Pts',(-2.37329561854466,0.186926755969883,3.63900200900026));
#8416=CARTESIAN_POINT('Ctrl Pts',(-2.37165914320747,0.0020537960080548,
3.65141010809498));
#8417=CARTESIAN_POINT('Ctrl Pts',(-2.37255724078598,0.00199178475905658,
2.84858989190502));
#8418=CARTESIAN_POINT('Ctrl Pts',(-2.36697397570993,-0.624252704055323,
2.89066247396608));
#8419=CARTESIAN_POINT('Ctrl Pts',(-1.79321255273579,-2.04018921676783,2.98518016125086));
#8420=CARTESIAN_POINT('Ctrl Pts',(0.584848394656438,-2.73293698550247,3.13214295375933));
#8421=CARTESIAN_POINT('Ctrl Pts',(2.60425579784155,-1.01431944186932,3.28947826943046));
#8422=CARTESIAN_POINT('Ctrl Pts',(2.27924634057658,1.61741407950708,3.44681358510158));
#8423=CARTESIAN_POINT('Ctrl Pts',(-0.0975982492034651,2.79311059143494,
3.6041489007727));
#8424=CARTESIAN_POINT('Ctrl Pts',(-2.04600507844241,1.65356799864077,3.73807433637385));
#8425=CARTESIAN_POINT('Ctrl Pts',(-2.36710223082098,0.433557734928271,3.81955466675129));
#8426=CARTESIAN_POINT('Ctrl Pts',(-2.36819322153198,-0.000653453332863235,
3.84858989190502));
#8427=CARTESIAN_POINT('Origin',(0.,0.,-1.84858989190501));
#8428=CARTESIAN_POINT('',(-2.36804188512505,-0.000112073902353324,1.65141010809498));
#8429=CARTESIAN_POINT('',(-2.37344137975612,-0.00178937704920473,1.84858989190502));
#8430=CARTESIAN_POINT('',(-2.37175,-1.78696459712734E-13,-1.84858989190501));
#8431=CARTESIAN_POINT('Ctrl Pts',(-2.36804188512505,-0.000112073902353224,
1.65141010809498));
#8432=CARTESIAN_POINT('Ctrl Pts',(-2.36821023678956,-0.384577180330964,
1.67711462161287));
#8433=CARTESIAN_POINT('Ctrl Pts',(-2.09930421630608,-1.55226751145704,1.75519863963526));
#8434=CARTESIAN_POINT('Ctrl Pts',(-0.275973625536248,-2.77999224892802,
1.88566216216216));
#8435=CARTESIAN_POINT('Ctrl Pts',(2.16802781286073,-1.76187209738162,2.04280067567567));
#8436=CARTESIAN_POINT('Ctrl Pts',(2.66479327803676,0.838697048159531,2.19993918918919));
#8437=CARTESIAN_POINT('Ctrl Pts',(0.76814623510466,2.68597898024514,2.3570777027027));
#8438=CARTESIAN_POINT('Ctrl Pts',(-1.70898688612053,2.14473275169325,2.50756800900463));
#8439=CARTESIAN_POINT('Ctrl Pts',(-2.36892240045369,0.678044518839718,2.60567881080206));
#8440=CARTESIAN_POINT('Ctrl Pts',(-2.37406517885066,-0.00153607482357281,
2.65141010809498));
#8441=CARTESIAN_POINT('Ctrl Pts',(-2.37344137975612,-0.00178937704920463,
1.84858989190502));
#8442=CARTESIAN_POINT('Ctrl Pts',(-2.37447812169567,-0.12506848067989,1.85688007073346));
#8443=CARTESIAN_POINT('Ctrl Pts',(-2.31006431944847,-1.02714724785255,1.91761535478561));
#8444=CARTESIAN_POINT('Ctrl Pts',(-1.15481219883121,-2.54507342378116,2.03079574406147));
#8445=CARTESIAN_POINT('Ctrl Pts',(1.49072764255621,-2.36404822464922,2.18813105973259));
#8446=CARTESIAN_POINT('Ctrl Pts',(2.79427705549031,-0.0548463935276453,
2.34546637540372));
#8447=CARTESIAN_POINT('Ctrl Pts',(1.5823475414007,2.30372918060613,2.50280169107483));
#8448=CARTESIAN_POINT('Ctrl Pts',(-1.05405113312049,2.58842974112365,2.66013700674597));
#8449=CARTESIAN_POINT('Ctrl Pts',(-2.29031280961247,1.08993341565411,2.77539974035602));
#8450=CARTESIAN_POINT('Ctrl Pts',(-2.37393373216083,0.15638533864836,2.83821736874238));
#8451=CARTESIAN_POINT('Ctrl Pts',(-2.37255724078598,0.00199178475905658,
2.84858989190502));
#8452=CARTESIAN_POINT('Origin',(0.,0.,-1.84858989190501));
#8453=CARTESIAN_POINT('',(-2.37366757034868,0.00184471646948807,0.651410108094983));
#8454=CARTESIAN_POINT('',(-2.36802324146013,0.000186122305323028,0.848589891905023));
#8455=CARTESIAN_POINT('',(-2.37175,-1.78696459712734E-13,-1.84858989190501));
#8456=CARTESIAN_POINT('Ctrl Pts',(-2.37366757034868,0.001844716469488,0.651410108094984));
#8457=CARTESIAN_POINT('Ctrl Pts',(-2.36827887140227,-0.663567421798888,
0.696170927919177));
#8458=CARTESIAN_POINT('Ctrl Pts',(-1.73206830317985,-2.11713322740477,0.793311252247876));
#8459=CARTESIAN_POINT('Ctrl Pts',(0.718910407331439,-2.69944634094777,0.942831081081078));
#8460=CARTESIAN_POINT('Ctrl Pts',(2.64899289676255,-0.887370898887054,1.09996959459459));
#8461=CARTESIAN_POINT('Ctrl Pts',(2.19990031581894,1.72195501972256,1.25710810810811));
#8462=CARTESIAN_POINT('Ctrl Pts',(-0.225079684819506,2.78455874530281,1.41424662162162));
#8463=CARTESIAN_POINT('Ctrl Pts',(-2.08428517335687,1.58152664346482,1.54568062161725));
#8464=CARTESIAN_POINT('Ctrl Pts',(-2.36786717732013,0.39886856587965,1.62473511710837));
#8465=CARTESIAN_POINT('Ctrl Pts',(-2.36804188512505,-0.000112073902353224,
1.65141010809498));
#8466=CARTESIAN_POINT('Ctrl Pts',(-2.36802324146013,0.000186122305323062,
0.848589891905023));
#8467=CARTESIAN_POINT('Ctrl Pts',(-2.36776001721126,-0.402962357372647,
0.87554277272455));
#8468=CARTESIAN_POINT('Ctrl Pts',(-2.0797505690667,-1.59092671500009,0.954940758767785));
#8469=CARTESIAN_POINT('Ctrl Pts',(-0.207121339063888,-2.78711087979173,
1.08678385003473));
#8470=CARTESIAN_POINT('Ctrl Pts',(2.21401803077907,-1.70561830406782,1.24411916570585));
#8471=CARTESIAN_POINT('Ctrl Pts',(2.64205485235054,0.911349150745493,1.40145448137697));
#8472=CARTESIAN_POINT('Ctrl Pts',(0.691640660298454,2.70787919402874,1.5587897970481));
#8473=CARTESIAN_POINT('Ctrl Pts',(-1.74582592441822,2.10050088985172,1.70783493389078));
#8474=CARTESIAN_POINT('Ctrl Pts',(-2.36791951286044,0.654816452515466,1.80443496550976));
#8475=CARTESIAN_POINT('Ctrl Pts',(-2.37344137975612,-0.00178937704920463,
1.84858989190502));
#8476=CARTESIAN_POINT('Origin',(0.,0.,11.5));
#8477=CARTESIAN_POINT('',(-2.86997293948595,0.000709208322249463,11.1339652973708));
#8478=CARTESIAN_POINT('Ctrl Pts',(-0.439445221994061,2.3306835819919,11.62825));
#8479=CARTESIAN_POINT('Ctrl Pts',(-0.359483020814685,2.34931149018937,11.6247602761445));
#8480=CARTESIAN_POINT('Ctrl Pts',(-0.27871400731898,2.36341693162049,11.6212847858384));
#8481=CARTESIAN_POINT('Ctrl Pts',(-0.197463562604575,2.37318447045242,11.6178187998135));
#8482=CARTESIAN_POINT('Ctrl Pts',(-0.114065564321399,2.38321017787593,11.614261203328));
#8483=CARTESIAN_POINT('Ctrl Pts',(-0.0301595928545948,2.38866567182183,
11.6107136201843));
#8484=CARTESIAN_POINT('Ctrl Pts',(0.0539178478306465,2.38969830818771,11.6071709361129));
#8485=CARTESIAN_POINT('Ctrl Pts',(0.0934462943689916,2.39018379527021,11.6055053668855));
#8486=CARTESIAN_POINT('Ctrl Pts',(0.133012786809523,2.38969093626847,11.6038408805234));
#8487=CARTESIAN_POINT('Ctrl Pts',(0.172582728329755,2.38823118545469,11.6021769455617));
#8488=CARTESIAN_POINT('Ctrl Pts',(0.196983674678661,2.38733102488025,11.6011508741002));
#8489=CARTESIAN_POINT('Ctrl Pts',(0.221385934120707,2.38606314465001,11.6001250123152));
#8490=CARTESIAN_POINT('Ctrl Pts',(0.24578137026875,2.38442977721171,11.5990992355836));
#8491=CARTESIAN_POINT('Ctrl Pts',(0.261730484740349,2.38336192320454,11.5984286088969));
#8492=CARTESIAN_POINT('Ctrl Pts',(0.277677591321838,2.38213767553654,11.597757980196));
#8493=CARTESIAN_POINT('Ctrl Pts',(0.293603734342933,2.38075929535175,11.5970880163414));
#8494=CARTESIAN_POINT('Ctrl Pts',(0.379341030417818,2.37333888038685,11.5934813119885));
#8495=CARTESIAN_POINT('Ctrl Pts',(0.464583014225527,2.36144918428767,11.5898891320915));
#8496=CARTESIAN_POINT('Ctrl Pts',(0.548977057540434,2.34525221307984,11.5863062427765));
#8497=CARTESIAN_POINT('Ctrl Pts',(0.63410785152571,2.32891384410355,11.5826920752337));
#8498=CARTESIAN_POINT('Ctrl Pts',(0.718376786391574,2.30819252148602,11.5790873611926));
#8499=CARTESIAN_POINT('Ctrl Pts',(0.801421129360431,2.28320149524268,11.5754867285058));
#8500=CARTESIAN_POINT('Ctrl Pts',(0.851520069054253,2.26812492443856,11.5733145410529));
#8501=CARTESIAN_POINT('Ctrl Pts',(0.901173245121242,2.25149340059607,11.5711438389925));
#8502=CARTESIAN_POINT('Ctrl Pts',(0.950298631716725,2.23332291784394,11.5689734428101));
#8503=CARTESIAN_POINT('Ctrl Pts',(0.963508179039198,2.22843697457875,11.5683898351671));
#8504=CARTESIAN_POINT('Ctrl Pts',(0.976678902975083,2.22343988211883,11.5678062771152));
#8505=CARTESIAN_POINT('Ctrl Pts',(0.989796896482515,2.2183369213822,11.5672232951128));
#8506=CARTESIAN_POINT('Ctrl Pts',(1.0715488401239,2.18653503351653,11.5635901242489));
#8507=CARTESIAN_POINT('Ctrl Pts',(1.15137916677557,2.15057972741051,11.5599737688071));
#8508=CARTESIAN_POINT('Ctrl Pts',(1.22892868995964,2.11061806082819,11.5563689172299));
#8509=CARTESIAN_POINT('Ctrl Pts',(1.30609743699769,2.07085261014462,11.5527817658451));
#8510=CARTESIAN_POINT('Ctrl Pts',(1.38100867140758,2.02711976610499,11.5492060056319));
#8511=CARTESIAN_POINT('Ctrl Pts',(1.45329568150197,1.97951483102432,11.5456364028898));
#8512=CARTESIAN_POINT('Ctrl Pts',(1.51120974849783,1.94137526215855,11.5427765500327));
#8513=CARTESIAN_POINT('Ctrl Pts',(1.56743935204678,1.90074932215926,11.5399206494764));
#8514=CARTESIAN_POINT('Ctrl Pts',(1.621783737959,1.85766460010194,11.5370660098083));
#8515=CARTESIAN_POINT('Ctrl Pts',(1.64895593091511,1.83612223907328,11.5356386899743));
#8516=CARTESIAN_POINT('Ctrl Pts',(1.67565661487015,1.81396489287275,11.5342116853624));
#8517=CARTESIAN_POINT('Ctrl Pts',(1.70185926132131,1.79119431574093,11.532784659546));
#8518=CARTESIAN_POINT('Ctrl Pts',(1.71882166156475,1.77645368090452,11.5318608680083));
#8519=CARTESIAN_POINT('Ctrl Pts',(1.73557532962421,1.76145603809249,11.5309370675846));
#8520=CARTESIAN_POINT('Ctrl Pts',(1.75211281381839,1.74620161928424,11.5300131670071));
#8521=CARTESIAN_POINT('Ctrl Pts',(1.76112158754248,1.73789179381609,11.529509873329));
#8522=CARTESIAN_POINT('Ctrl Pts',(1.77006808708219,1.72950393138366,11.5290064421071));
#8523=CARTESIAN_POINT('Ctrl Pts',(1.77894146971999,1.72104732904951,11.5285034067769));
#8524=CARTESIAN_POINT('Ctrl Pts',(1.83933200754334,1.66349331791721,11.5250798449438));
#8525=CARTESIAN_POINT('Ctrl Pts',(1.8963984276916,1.60270624192685,11.5216713230637));
#8526=CARTESIAN_POINT('Ctrl Pts',(1.95011819953022,1.53907807970147,11.5182734051049));
#8527=CARTESIAN_POINT('Ctrl Pts',(2.00542449571231,1.47357076525995,11.5147751352761));
#8528=CARTESIAN_POINT('Ctrl Pts',(2.05718398574646,1.40505149787053,11.511288104956));
#8529=CARTESIAN_POINT('Ctrl Pts',(2.10533946111886,1.3339039115796,11.5078074733588));
#8530=CARTESIAN_POINT('Ctrl Pts',(2.15154257592138,1.26564085173229,11.5044679565119));
#8531=CARTESIAN_POINT('Ctrl Pts',(2.19442802485129,1.19495736996561,11.5011343300606));
#8532=CARTESIAN_POINT('Ctrl Pts',(2.23391281993103,1.12216394079048,11.4978023184486));
#8533=CARTESIAN_POINT('Ctrl Pts',(2.25118741777841,1.09031681552637,11.4963445633684));
#8534=CARTESIAN_POINT('Ctrl Pts',(2.26781067606573,1.05806553560368,11.4948871173785));
#8535=CARTESIAN_POINT('Ctrl Pts',(2.28377353610697,1.02543493097626,11.4934296224428));
#8536=CARTESIAN_POINT('Ctrl Pts',(2.29326703470383,1.00602872191068,11.4925628149854));
#8537=CARTESIAN_POINT('Ctrl Pts',(2.30252692730832,0.986488335264957,11.4916959902159));
#8538=CARTESIAN_POINT('Ctrl Pts',(2.31155107931692,0.966818908506685,11.4908290728209));
#8539=CARTESIAN_POINT('Ctrl Pts',(2.31863529945096,0.951377840034761,11.490148517611));
#8540=CARTESIAN_POINT('Ctrl Pts',(2.32557538886546,0.935854346809815,11.4894677807698));
#8541=CARTESIAN_POINT('Ctrl Pts',(2.33236053374086,0.920273937348818,11.4887878255595));
#8542=CARTESIAN_POINT('Ctrl Pts',(2.36796902716184,0.838507826532316,11.4852194152932));
#8543=CARTESIAN_POINT('Ctrl Pts',(2.39937221583678,0.755052917299449,11.4816670269197));
#8544=CARTESIAN_POINT('Ctrl Pts',(2.42650990964853,0.670313949715511,11.4781256336386));
#8545=CARTESIAN_POINT('Ctrl Pts',(2.45395171326163,0.584625382258507,11.4745445548773));
#8546=CARTESIAN_POINT('Ctrl Pts',(2.47703230477293,0.497622920338958,11.470974719015));
#8547=CARTESIAN_POINT('Ctrl Pts',(2.49564463758615,0.409696684762178,11.4674109283565));
#8548=CARTESIAN_POINT('Ctrl Pts',(2.51256694354607,0.329754279086013,11.464170735066));
#8549=CARTESIAN_POINT('Ctrl Pts',(2.52579526118549,0.24904737731457,11.460935538995));
#8550=CARTESIAN_POINT('Ctrl Pts',(2.53521313973642,0.167858755145902,11.4577014336506));
#8551=CARTESIAN_POINT('Ctrl Pts',(2.53942638325848,0.131537684050459,11.4562546032081));
#8552=CARTESIAN_POINT('Ctrl Pts',(2.54287653840534,0.0951201284473648,11.4548079910601));
#8553=CARTESIAN_POINT('Ctrl Pts',(2.54555076253572,0.0586312673898904,11.4533612474409));
#8554=CARTESIAN_POINT('Ctrl Pts',(2.54678080763582,0.0418477284777441,11.4526957983935));
#8555=CARTESIAN_POINT('Ctrl Pts',(2.54784667039524,0.0250491043820508,11.4520303215313));
#8556=CARTESIAN_POINT('Ctrl Pts',(2.54874698931854,0.00823785327091157,
11.4513647828174));
#8557=CARTESIAN_POINT('Ctrl Pts',(2.54950258918657,-0.00587112388394168,
11.4508062241208));
#8558=CARTESIAN_POINT('Ctrl Pts',(2.55014158604825,-0.0199907301096276,
11.4502475533557));
#8559=CARTESIAN_POINT('Ctrl Pts',(2.55066270854233,-0.0341027028361791,
11.4496894146469));
#8560=CARTESIAN_POINT('Ctrl Pts',(2.55400035119776,-0.124485909584641,11.4461146935723));
#8561=CARTESIAN_POINT('Ctrl Pts',(2.55251590030915,-0.214700787372498,11.4425560101414));
#8562=CARTESIAN_POINT('Ctrl Pts',(2.54610973516166,-0.304360270645855,11.4390083150826));
#8563=CARTESIAN_POINT('Ctrl Pts',(2.53992350143221,-0.390941635131681,11.4355824166973));
#8564=CARTESIAN_POINT('Ctrl Pts',(2.52914771427487,-0.477005973362024,11.4321667651471));
#8565=CARTESIAN_POINT('Ctrl Pts',(2.51364702202946,-0.56221151242787,11.4287568135539));
#8566=CARTESIAN_POINT('Ctrl Pts',(2.4978416408886,-0.649091891634602,11.4252798343488));
#8567=CARTESIAN_POINT('Ctrl Pts',(2.47712400969773,-0.735080204165537,11.4218087813851));
#8568=CARTESIAN_POINT('Ctrl Pts',(2.45176245019841,-0.819915179815436,11.4183388343531));
#8569=CARTESIAN_POINT('Ctrl Pts',(2.43759878319083,-0.867292958210081,11.4164009734618));
#8570=CARTESIAN_POINT('Ctrl Pts',(2.42198578511571,-0.914310849766526,11.4144634574981));
#8571=CARTESIAN_POINT('Ctrl Pts',(2.40496360252248,-0.960921226687823,11.4125254468584));
#8572=CARTESIAN_POINT('Ctrl Pts',(2.39839032938233,-0.978920254544038,11.4117770661373));
#8573=CARTESIAN_POINT('Ctrl Pts',(2.39160484182306,-0.996863365779891,11.4110284061025));
#8574=CARTESIAN_POINT('Ctrl Pts',(2.38462104532031,-1.01471861919519,11.4102806421704));
#8575=CARTESIAN_POINT('Ctrl Pts',(2.35196925304181,-1.09819843212604,11.4067845734384));
#8576=CARTESIAN_POINT('Ctrl Pts',(2.31495075727319,-1.17986515814379,11.4033036769767));
#8577=CARTESIAN_POINT('Ctrl Pts',(2.27389075093231,-1.25946542646749,11.3998332297369));
#8578=CARTESIAN_POINT('Ctrl Pts',(2.23207387867294,-1.34053297976178,11.3962988111666));
#8579=CARTESIAN_POINT('Ctrl Pts',(2.18606471254661,-1.41945796930655,11.3927752305933));
#8580=CARTESIAN_POINT('Ctrl Pts',(2.13615274225743,-1.49596025824322,11.3892574989426));
#8581=CARTESIAN_POINT('Ctrl Pts',(2.08602408315185,-1.57279467573233,11.385724495342));
#8582=CARTESIAN_POINT('Ctrl Pts',(2.03195810671375,-1.64718611516111,11.3821973915595));
#8583=CARTESIAN_POINT('Ctrl Pts',(1.97420160691916,-1.71882633760539,11.3786711332592));
#8584=CARTESIAN_POINT('Ctrl Pts',(1.95240508667088,-1.74586238661548,11.377340371168));
#8585=CARTESIAN_POINT('Ctrl Pts',(1.93008253152955,-1.77250629512415,11.3760097294909));
#8586=CARTESIAN_POINT('Ctrl Pts',(1.90724574604483,-1.79874022848494,11.3746789365696));
#8587=CARTESIAN_POINT('Ctrl Pts',(1.89585779635524,-1.81182222347379,11.3740153141501));
#8588=CARTESIAN_POINT('Ctrl Pts',(1.8843419621495,-1.82480225835256,11.3733516541209));
#8589=CARTESIAN_POINT('Ctrl Pts',(1.87269964124851,-1.83767804526001,11.3726879227956));
#8590=CARTESIAN_POINT('Ctrl Pts',(1.86326625859819,-1.8481108640987,11.3721501235353));
#8591=CARTESIAN_POINT('Ctrl Pts',(1.8537496389451,-1.8584753407347,11.3716122696922));
#8592=CARTESIAN_POINT('Ctrl Pts',(1.8441608279676,-1.86875948192732,11.3710749125616));
#8593=CARTESIAN_POINT('Ctrl Pts',(1.78056218360928,-1.93696996597738,11.3675108434478));
#8594=CARTESIAN_POINT('Ctrl Pts',(1.71368420494736,-2.00176842633816,11.3639624618779));
#8595=CARTESIAN_POINT('Ctrl Pts',(1.64382533951827,-2.06287172496906,11.3604247664903));
#8596=CARTESIAN_POINT('Ctrl Pts',(1.57423141411002,-2.12374328910052,11.3569004878264));
#8597=CARTESIAN_POINT('Ctrl Pts',(1.50167852811227,-2.18094842953722,11.3533868144436));
#8598=CARTESIAN_POINT('Ctrl Pts',(1.42641996197867,-2.2341772386581,11.3498788016679));
#8599=CARTESIAN_POINT('Ctrl Pts',(1.3516762241841,-2.28704192046701,11.3463947864845));
#8600=CARTESIAN_POINT('Ctrl Pts',(1.27426307539374,-2.33598522008376,11.342916354727));
#8601=CARTESIAN_POINT('Ctrl Pts',(1.19439676647842,-2.38066281826916,11.339438662505));
#8602=CARTESIAN_POINT('Ctrl Pts',(1.15339338620205,-2.40360030684365,11.3376532145659));
#8603=CARTESIAN_POINT('Ctrl Pts',(1.11174294293827,-2.42541271468527,11.3358679615534));
#8604=CARTESIAN_POINT('Ctrl Pts',(1.06947220915485,-2.44604826098259,11.334082247983));
#8605=CARTESIAN_POINT('Ctrl Pts',(1.05124776879456,-2.45494499044852,11.3333123623541));
#8606=CARTESIAN_POINT('Ctrl Pts',(1.0329023157667,-2.46362538871231,11.3325421557385));
#8607=CARTESIAN_POINT('Ctrl Pts',(1.01446903163988,-2.47207123914098,11.3317728670993));
#8608=CARTESIAN_POINT('Ctrl Pts',(0.992379075227472,-2.48219252119531,11.3308509720972));
#8609=CARTESIAN_POINT('Ctrl Pts',(0.970156538466361,-2.49198036655811,11.3299301186847));
#8610=CARTESIAN_POINT('Ctrl Pts',(0.94780620569595,-2.50142961190602,11.3290102203308));
#8611=CARTESIAN_POINT('Ctrl Pts',(0.865790439448149,-2.53610413356231,11.3256346031023));
#8612=CARTESIAN_POINT('Ctrl Pts',(0.78205610317221,-2.56622272676918,11.3222718463403));
#8613=CARTESIAN_POINT('Ctrl Pts',(0.696974578785958,-2.59191739767486,11.318917674299));
#8614=CARTESIAN_POINT('Ctrl Pts',(0.609579162327931,-2.61831086536073,11.3154722816062));
#8615=CARTESIAN_POINT('Ctrl Pts',(0.520761565645775,-2.64003666842693,11.3120359469267));
#8616=CARTESIAN_POINT('Ctrl Pts',(0.430899300361841,-2.65718927641842,11.3086040360895));
#8617=CARTESIAN_POINT('Ctrl Pts',(0.343209845834361,-2.67392714557567,11.3052551066101));
#8618=CARTESIAN_POINT('Ctrl Pts',(0.25452479015491,-2.6863100783274,11.3019103896282));
#8619=CARTESIAN_POINT('Ctrl Pts',(0.165183352753207,-2.69438132192965,11.2985655790638));
#8620=CARTESIAN_POINT('Ctrl Pts',(0.137834848150192,-2.69685202812409,11.2975416917191));
#8621=CARTESIAN_POINT('Ctrl Pts',(0.110424801620538,-2.69891839950379,11.2965177956053));
#8622=CARTESIAN_POINT('Ctrl Pts',(0.08296290180991,-2.70058085938097,11.2954937672061));
#8623=CARTESIAN_POINT('Ctrl Pts',(0.0669684788561147,-2.70154911309258,
11.2948973502268));
#8624=CARTESIAN_POINT('Ctrl Pts',(0.0509564666454086,-2.70238034652659,
11.2943008883741));
#8625=CARTESIAN_POINT('Ctrl Pts',(0.0349287839010169,-2.70307458363613,
11.2937043572455));
#8626=CARTESIAN_POINT('Ctrl Pts',(0.0206834334719444,-2.70369161924033,
11.293174162388));
#8627=CARTESIAN_POINT('Ctrl Pts',(0.00643409067270473,-2.70420004997344,
11.2926442249703));
#8628=CARTESIAN_POINT('Ctrl Pts',(-0.00781400179505987,-2.70460019597085,
11.2921146711228));
#8629=CARTESIAN_POINT('Ctrl Pts',(-0.101952151334104,-2.70724398873305,
11.2886158715889));
#8630=CARTESIAN_POINT('Ctrl Pts',(-0.196088226677417,-2.7051673117304,11.2851318105594));
#8631=CARTESIAN_POINT('Ctrl Pts',(-0.289825667638303,-2.6984813516168,11.2816577549713));
#8632=CARTESIAN_POINT('Ctrl Pts',(-0.384631538117472,-2.69171918420471,
11.2781441017209));
#8633=CARTESIAN_POINT('Ctrl Pts',(-0.479030586990251,-2.68024208441543,
11.2746406832979));
#8634=CARTESIAN_POINT('Ctrl Pts',(-0.57262152425153,-2.66411259564997,11.2711426029439));
#8635=CARTESIAN_POINT('Ctrl Pts',(-0.666559717691804,-2.64792326065578,
11.2676315434484));
#8636=CARTESIAN_POINT('Ctrl Pts',(-0.759684799865766,-2.62704692522732,
11.2641258617076));
#8637=CARTESIAN_POINT('Ctrl Pts',(-0.851585181919148,-2.6014943492988,11.2606206062542));
#8638=CARTESIAN_POINT('Ctrl Pts',(-0.886047825189167,-2.59191213332561,
11.2593061354592));
#8639=CARTESIAN_POINT('Ctrl Pts',(-0.920338108563248,-2.58167179563189,
11.2579917246108));
#8640=CARTESIAN_POINT('Ctrl Pts',(-0.95443366677234,-2.57077201863537,11.2566771125966));
#8641=CARTESIAN_POINT('Ctrl Pts',(-0.974280480974564,-2.5644273256531,11.255911885049));
#8642=CARTESIAN_POINT('Ctrl Pts',(-0.99406130744013,-2.55785917358927,11.2551465893396));
#8643=CARTESIAN_POINT('Ctrl Pts',(-1.01377165408274,-2.55106714297751,11.2543811739687));
#8644=CARTESIAN_POINT('Ctrl Pts',(-1.02736841414217,-2.54638180627496,11.2538531685848));
#8645=CARTESIAN_POINT('Ctrl Pts',(-1.04092225787931,-2.54159315279905,11.253325470206));
#8646=CARTESIAN_POINT('Ctrl Pts',(-1.05443025528497,-2.53670205395909,11.252798124302));
#8647=CARTESIAN_POINT('Ctrl Pts',(-1.14463510839177,-2.50403985843604,11.2492765690056));
#8648=CARTESIAN_POINT('Ctrl Pts',(-1.23281912858369,-2.46680540724472,11.2457698275395));
#8649=CARTESIAN_POINT('Ctrl Pts',(-1.31858159439492,-2.42506535814129,11.242273074989));
#8650=CARTESIAN_POINT('Ctrl Pts',(-1.40311199337542,-2.38392494816353,11.2388265569179));
#8651=CARTESIAN_POINT('Ctrl Pts',(-1.48529083212456,-2.33840727081253,11.2353897428216));
#8652=CARTESIAN_POINT('Ctrl Pts',(-1.56472199239298,-2.28852750879454,11.2319580127567));
#8653=CARTESIAN_POINT('Ctrl Pts',(-1.58551758994019,-2.27546866069046,11.2310595633688));
#8654=CARTESIAN_POINT('Ctrl Pts',(-1.60612474663732,-2.26211056997792,11.230161462454));
#8655=CARTESIAN_POINT('Ctrl Pts',(-1.62653609083598,-2.2484529714829,11.2292636271078));
#8656=CARTESIAN_POINT('Ctrl Pts',(-1.70441968299709,-2.19633965543995,11.225837755629));
#8657=CARTESIAN_POINT('Ctrl Pts',(-1.77945485532057,-2.13986885585993,11.222415750716));
#8658=CARTESIAN_POINT('Ctrl Pts',(-1.85149349468849,-2.07939019092048,11.2189930066095));
#8659=CARTESIAN_POINT('Ctrl Pts',(-1.8748645479439,-2.05976946915896,11.2178825867641));
#8660=CARTESIAN_POINT('Ctrl Pts',(-1.89791995295043,-2.03972659946025,11.2167720891179));
#8661=CARTESIAN_POINT('Ctrl Pts',(-1.92065386067013,-2.01927267290743,11.2156613564032));
#8662=CARTESIAN_POINT('Ctrl Pts',(-1.9316413592642,-2.00938710936888,11.2151245294621));
#8663=CARTESIAN_POINT('Ctrl Pts',(-1.94255421950186,-1.99940498570623,11.2145876221361));
#8664=CARTESIAN_POINT('Ctrl Pts',(-1.95338011991677,-1.98933864610605,11.2140511999421));
#8665=CARTESIAN_POINT('Ctrl Pts',(-2.02242773931489,-1.92513550744723,11.2106298978731));
#8666=CARTESIAN_POINT('Ctrl Pts',(-2.08805585991204,-1.85740773886018,11.2072227031525));
#8667=CARTESIAN_POINT('Ctrl Pts',(-2.15015903930769,-1.7865606665237,11.2038251982962));
#8668=CARTESIAN_POINT('Ctrl Pts',(-2.21349481278046,-1.71430745552261,11.2003602613952));
#8669=CARTESIAN_POINT('Ctrl Pts',(-2.27316487566809,-1.63880924004706,11.1969054028151));
#8670=CARTESIAN_POINT('Ctrl Pts',(-2.32902567586957,-1.56045035084564,11.1934559367882));
#8671=CARTESIAN_POINT('Ctrl Pts',(-2.38527990190259,-1.48153958249049,11.1899821762823));
#8672=CARTESIAN_POINT('Ctrl Pts',(-2.43767154642151,-1.39972691196139,11.1865138845562));
#8673=CARTESIAN_POINT('Ctrl Pts',(-2.48601414345046,-1.31537014370798,11.1830462761383));
#8674=CARTESIAN_POINT('Ctrl Pts',(-2.51324863986033,-1.26784654664574,11.1810927491288));
#8675=CARTESIAN_POINT('Ctrl Pts',(-2.53919729042327,-1.21951494628862,11.1791394389872));
#8676=CARTESIAN_POINT('Ctrl Pts',(-2.56382026308967,-1.17043597842562,11.1771854900701));
#8677=CARTESIAN_POINT('Ctrl Pts',(-2.57043915220293,-1.15724308533024,11.1766602500274));
#8678=CARTESIAN_POINT('Ctrl Pts',(-2.57696321367054,-1.1439941193146,11.1761348825453));
#8679=CARTESIAN_POINT('Ctrl Pts',(-2.58338840616944,-1.13069688731366,11.175609633533));
#8680=CARTESIAN_POINT('Ctrl Pts',(-2.62620034331217,-1.04209561027884,11.172109827464));
#8681=CARTESIAN_POINT('Ctrl Pts',(-2.66450788394824,-0.951602474453648,
11.1686250464566));
#8682=CARTESIAN_POINT('Ctrl Pts',(-2.69817002472794,-0.859613847080416,
11.1651505728457));
#8683=CARTESIAN_POINT('Ctrl Pts',(-2.73183382450822,-0.767620686151626,
11.1616759279993));
#8684=CARTESIAN_POINT('Ctrl Pts',(-2.76085223666098,-0.67413102162785,11.1582115915653));
#8685=CARTESIAN_POINT('Ctrl Pts',(-2.78504109696179,-0.579512179774996,
11.1547528451809));
#8686=CARTESIAN_POINT('Ctrl Pts',(-2.80867562760501,-0.487061692675289,
11.1513733619645));
#8687=CARTESIAN_POINT('Ctrl Pts',(-2.8276996967141,-0.393532337548253,11.1479992155222));
#8688=CARTESIAN_POINT('Ctrl Pts',(-2.84189514122644,-0.299251761426908,
11.1446260045022));
#8689=CARTESIAN_POINT('Ctrl Pts',(-2.85324010443846,-0.223902964369238,
11.1419301428196));
#8690=CARTESIAN_POINT('Ctrl Pts',(-2.86150015598816,-0.148073915036915,
11.1392348786069));
#8691=CARTESIAN_POINT('Ctrl Pts',(-2.86653995619031,-0.0719300717664526,
11.1365379651471));
#8692=CARTESIAN_POINT('Ctrl Pts',(-2.86814414143213,-0.0476932320643782,
11.1356795285827));
#8693=CARTESIAN_POINT('Ctrl Pts',(-2.86941988081495,-0.0234547494955555,
11.1348219958471));
#8694=CARTESIAN_POINT('Ctrl Pts',(-2.87036479087719,0.000779773978368722,
11.1339652973708));
#8695=CARTESIAN_POINT('',(0.261199069988913,2.92594434598213,11.058));
#8696=CARTESIAN_POINT('Ctrl Pts',(0.261124777554784,2.92529416030266,11.058));
#8697=CARTESIAN_POINT('Ctrl Pts',(0.163252076286772,2.9214051496811,11.0703793245688));
#8698=CARTESIAN_POINT('Ctrl Pts',(0.0658388360676064,2.91286361031638,11.0828028087884));
#8699=CARTESIAN_POINT('Ctrl Pts',(-0.0307369711720644,2.89968653111402,
11.0952900032599));
#8700=CARTESIAN_POINT('Ctrl Pts',(-0.12623809978967,2.88665608413482,11.1076382424244));
#8701=CARTESIAN_POINT('Ctrl Pts',(-0.220921197195477,2.86909236615812,11.1200487818169));
#8702=CARTESIAN_POINT('Ctrl Pts',(-0.31439997383375,2.84696555496448,11.1325405266072));
#8703=CARTESIAN_POINT('Ctrl Pts',(-0.389995520831668,2.82907177783499,11.1426425017756));
#8704=CARTESIAN_POINT('Ctrl Pts',(-0.464803253647579,2.80819289824412,11.152797583885));
#8705=CARTESIAN_POINT('Ctrl Pts',(-0.538603048202427,2.78429272567688,11.1630157713274));
#8706=CARTESIAN_POINT('Ctrl Pts',(-0.593952894118562,2.76636759625145,11.1706794119091));
#8707=CARTESIAN_POINT('Ctrl Pts',(-0.648735503576454,2.7467426089957,11.1783785492407));
#8708=CARTESIAN_POINT('Ctrl Pts',(-0.702851172581185,2.72539620337798,11.1861174013937));
#8709=CARTESIAN_POINT('Ctrl Pts',(-0.71873840261759,2.71912934457837,11.1883893667345));
#8710=CARTESIAN_POINT('Ctrl Pts',(-0.734568107078247,2.71271408483162,11.190664755044));
#8711=CARTESIAN_POINT('Ctrl Pts',(-0.750337652372167,2.70614979460715,11.1929436730527));
#8712=CARTESIAN_POINT('Ctrl Pts',(-0.763539656096334,2.70065427889159,11.1948515456945));
#8713=CARTESIAN_POINT('Ctrl Pts',(-0.776691326847496,2.69505769580723,11.1967607130315));
#8714=CARTESIAN_POINT('Ctrl Pts',(-0.789788993683481,2.68936106997679,11.1986708957826));
#8715=CARTESIAN_POINT('Ctrl Pts',(-0.87317349082548,2.65309428397392,11.2108318119326));
#8716=CARTESIAN_POINT('Ctrl Pts',(-0.954403883416443,2.61276259333994,11.2230385405707));
#8717=CARTESIAN_POINT('Ctrl Pts',(-1.03314628688233,2.56834468618871,11.2353100289649));
#8718=CARTESIAN_POINT('Ctrl Pts',(-1.07823214235908,2.54291214597843,11.2423363645588));
#8719=CARTESIAN_POINT('Ctrl Pts',(-1.12250179725942,2.51613922516579,11.2493839310575));
#8720=CARTESIAN_POINT('Ctrl Pts',(-1.16588734321926,2.48801620495338,11.2564562851141));
#8721=CARTESIAN_POINT('Ctrl Pts',(-1.2435976078222,2.43764349916415,11.2691239718505));
#8722=CARTESIAN_POINT('Ctrl Pts',(-1.31847408700313,2.38294042952196,11.2818711829841));
#8723=CARTESIAN_POINT('Ctrl Pts',(-1.39030087935118,2.32423346489716,11.2947183566611));
#8724=CARTESIAN_POINT('Ctrl Pts',(-1.46342993694969,2.26446210581046,11.3077984577361));
#8725=CARTESIAN_POINT('Ctrl Pts',(-1.53339828473794,2.20053932645019,11.3209821789827));
#8726=CARTESIAN_POINT('Ctrl Pts',(-1.59992558939365,2.1327921427514,11.3342910904939));
#8727=CARTESIAN_POINT('Ctrl Pts',(-1.61340208445737,2.11906853570881,11.3369870884937));
#8728=CARTESIAN_POINT('Ctrl Pts',(-1.62674073455187,2.10518403555254,11.3396889690338));
#8729=CARTESIAN_POINT('Ctrl Pts',(-1.63991787601809,2.09116421105248,11.3423925384684));
#8730=CARTESIAN_POINT('Ctrl Pts',(-1.70139884650346,2.02575150993609,11.3550066606613));
#8731=CARTESIAN_POINT('Ctrl Pts',(-1.75944768512028,1.95731714657644,11.3676731670409));
#8732=CARTESIAN_POINT('Ctrl Pts',(-1.8138993651727,1.88618389956551,11.3804137020214));
#8733=CARTESIAN_POINT('Ctrl Pts',(-1.86815753562372,1.81530344486993,11.393108959871));
#8734=CARTESIAN_POINT('Ctrl Pts',(-1.91884436205444,1.74174225535381,11.4058777210929));
#8735=CARTESIAN_POINT('Ctrl Pts',(-1.96574838356875,1.66580180077525,11.4187414001618));
#8736=CARTESIAN_POINT('Ctrl Pts',(-2.01186212788083,1.59114085290088,11.4313883414761));
#8737=CARTESIAN_POINT('Ctrl Pts',(-2.05431959945996,1.51417923664983,11.4441270290762));
#8738=CARTESIAN_POINT('Ctrl Pts',(-2.09287020326133,1.43520021222363,11.4569778131465));
#8739=CARTESIAN_POINT('Ctrl Pts',(-2.11361694660402,1.39269614256837,11.4638937079073));
#8740=CARTESIAN_POINT('Ctrl Pts',(-2.13323129045024,1.34960780406157,11.4708420687169));
#8741=CARTESIAN_POINT('Ctrl Pts',(-2.15166787184208,1.30598030868302,11.4778260675126));
#8742=CARTESIAN_POINT('Ctrl Pts',(-2.15713184571921,1.29305060712901,11.4798958865407));
#8743=CARTESIAN_POINT('Ctrl Pts',(-2.16249308944786,1.28007170317631,11.4819691313049));
#8744=CARTESIAN_POINT('Ctrl Pts',(-2.16774797314523,1.26705068510794,11.4840449452013));
#8745=CARTESIAN_POINT('Ctrl Pts',(-2.19963752356477,1.18803192158837,11.4966421358759));
#8746=CARTESIAN_POINT('Ctrl Pts',(-2.22751419897903,1.10771397257159,11.5092939385505));
#8747=CARTESIAN_POINT('Ctrl Pts',(-2.25120331746379,1.02636717479289,11.5220225137828));
#8748=CARTESIAN_POINT('Ctrl Pts',(-2.27454503464211,0.946213329121761,11.5345644242532));
#8749=CARTESIAN_POINT('Ctrl Pts',(-2.29382118362004,0.865059764231561,11.5471808720505));
#8750=CARTESIAN_POINT('Ctrl Pts',(-2.30881496364231,0.783166675687281,11.5598930570057));
#8751=CARTESIAN_POINT('Ctrl Pts',(-2.3233692591387,0.703673965509062,11.572232633548));
#8752=CARTESIAN_POINT('Ctrl Pts',(-2.33388845327117,0.623483808186223,11.5846624171728));
#8753=CARTESIAN_POINT('Ctrl Pts',(-2.34012749274977,0.542846284442329,11.5972017976454));
#8754=CARTESIAN_POINT('Ctrl Pts',(-2.34523853245788,0.476787785015864,11.6074740954455));
#8755=CARTESIAN_POINT('Ctrl Pts',(-2.34747636127652,0.410429125649976,11.6178199429796));
#8756=CARTESIAN_POINT('Ctrl Pts',(-2.34668236863853,0.343918483395475,11.62825));
#8757=CARTESIAN_POINT('',(-2.14415473270599,2.01243073062329,11.058));
#8758=CARTESIAN_POINT('Origin',(0.,0.,11.058));
#8759=CARTESIAN_POINT('Ctrl Pts',(-2.87036479087719,0.000779773978368722,
11.1339652973708));
#8760=CARTESIAN_POINT('Ctrl Pts',(-2.87200285191233,0.0427918449624727,
11.1324801566689));
#8761=CARTESIAN_POINT('Ctrl Pts',(-2.87264678506693,0.0847919926152422,
11.1309975229776));
#8762=CARTESIAN_POINT('Ctrl Pts',(-2.87228289058568,0.126751532711213,11.1295170338848));
#8763=CARTESIAN_POINT('Ctrl Pts',(-2.87145802595519,0.221864106052536,11.1261611075067));
#8764=CARTESIAN_POINT('Ctrl Pts',(-2.86545855469524,0.316767622116373,11.1228162005919));
#8765=CARTESIAN_POINT('Ctrl Pts',(-2.85455763680452,0.411156736693552,11.1194780920563));
#8766=CARTESIAN_POINT('Ctrl Pts',(-2.84342076253498,0.507588955704657,11.1160677283208));
#8767=CARTESIAN_POINT('Ctrl Pts',(-2.82716775830471,0.603485022278454,11.1126644604589));
#8768=CARTESIAN_POINT('Ctrl Pts',(-2.80603441756026,0.698520670355508,11.1092637873076));
#8769=CARTESIAN_POINT('Ctrl Pts',(-2.79266006313991,0.75866451866233,11.1071116520374));
#8770=CARTESIAN_POINT('Ctrl Pts',(-2.77733000149192,0.818463754777881,11.1049605559651));
#8771=CARTESIAN_POINT('Ctrl Pts',(-2.76009348614301,0.877834296726592,11.1028093582138));
#8772=CARTESIAN_POINT('Ctrl Pts',(-2.74919109087412,0.915387195473845,11.1014486882808));
#8773=CARTESIAN_POINT('Ctrl Pts',(-2.73752580613221,0.952768545576029,11.1000879776682));
#8774=CARTESIAN_POINT('Ctrl Pts',(-2.72510854264357,0.989956497598032,11.0987269376699));
#8775=CARTESIAN_POINT('Ctrl Pts',(-2.72027063675402,1.00444534308902,11.0981966611375));
#8776=CARTESIAN_POINT('Ctrl Pts',(-2.71531799003855,1.0189064745382,11.0976662739811));
#8777=CARTESIAN_POINT('Ctrl Pts',(-2.71025302608607,1.03333338889234,11.0971359498549));
#8778=CARTESIAN_POINT('Ctrl Pts',(-2.67741979989202,1.12685471435798,11.0936981658637));
#8779=CARTESIAN_POINT('Ctrl Pts',(-2.63998428261572,1.2186200392303,11.0902747408666));
#8780=CARTESIAN_POINT('Ctrl Pts',(-2.59822193704792,1.30830487286322,11.0868612068006));
#8781=CARTESIAN_POINT('Ctrl Pts',(-2.55598691495593,1.39900478155616,11.0834090375144));
#8782=CARTESIAN_POINT('Ctrl Pts',(-2.50932621498891,1.48757769234242,11.0799669843223));
#8783=CARTESIAN_POINT('Ctrl Pts',(-2.45847158858181,1.57367848927911,11.0765304257261));
#8784=CARTESIAN_POINT('Ctrl Pts',(-2.40788866695146,1.65931926911486,11.0731122278858));
#8785=CARTESIAN_POINT('Ctrl Pts',(-2.35315604081231,1.74251510638125,11.0696994660854));
#8786=CARTESIAN_POINT('Ctrl Pts',(-2.29445585803367,1.82290449738493,11.0662875925062));
#8787=CARTESIAN_POINT('Ctrl Pts',(-2.24693123162509,1.88798906090443,11.0635252839489));
#8788=CARTESIAN_POINT('Ctrl Pts',(-2.19680500482205,1.95123384018432,11.0607635576017));
#8789=CARTESIAN_POINT('Ctrl Pts',(-2.14415473270599,2.01243073062329,11.058));
#8790=CARTESIAN_POINT('',(-2.,-2.4492935982947E-16,12.));
#8791=CARTESIAN_POINT('',(-2.5,-3.06161699786838E-16,11.5));
#8792=CARTESIAN_POINT('Origin',(0.,0.,12.));
#8793=CARTESIAN_POINT('Ctrl Pts',(1.70810875200395,-2.39535560853238,-0.329233991005387));
#8794=CARTESIAN_POINT('Ctrl Pts',(2.49644455514999,-1.833199709811,-0.276854486500882));
#8795=CARTESIAN_POINT('Ctrl Pts',(3.46233357982621,0.120022568706166,-0.172095477491873));
#8796=CARTESIAN_POINT('Ctrl Pts',(1.80423238277522,2.96114098648209,-0.0149569639783592));
#8797=CARTESIAN_POINT('Ctrl Pts',(-1.47579564172449,3.13432118289611,0.142181549535154));
#8798=CARTESIAN_POINT('Ctrl Pts',(-3.42956675747562,0.496557026061836,0.299320063048668));
#8799=CARTESIAN_POINT('Ctrl Pts',(-2.30343226514234,-2.58935922774548,0.456458576562181));
#8800=CARTESIAN_POINT('Ctrl Pts',(0.891761112414455,-3.34848577424617,0.613597090075694));
#8801=CARTESIAN_POINT('Ctrl Pts',(3.2859015926111,-1.1007252807108,0.770735603589207));
#8802=CARTESIAN_POINT('Ctrl Pts',(2.7288317609948,2.13597203247546,0.927874117102722));
#8803=CARTESIAN_POINT('Ctrl Pts',(-0.27919655644097,3.45406211813255,1.08501263061624));
#8804=CARTESIAN_POINT('Ctrl Pts',(-3.03644606033952,1.66993460430069,1.24215114412975));
#8805=CARTESIAN_POINT('Ctrl Pts',(-3.06648780987738,-1.61410638094873,1.39928965764326));
#8806=CARTESIAN_POINT('Ctrl Pts',(-0.342327145073366,-3.44839767949667,
1.55642817115678));
#8807=CARTESIAN_POINT('Ctrl Pts',(2.68929601578421,-2.18548654390084,1.71356668467029));
#8808=CARTESIAN_POINT('Ctrl Pts',(3.30550092715682,1.04034856780235,1.8707051981838));
#8809=CARTESIAN_POINT('Ctrl Pts',(0.952834920914103,3.33178039838987,2.02784371169731));
#8810=CARTESIAN_POINT('Ctrl Pts',(-2.25562944112346,2.630740466173,2.18498222521083));
#8811=CARTESIAN_POINT('Ctrl Pts',(-3.43817673987435,-0.433127500149091,
2.34212073872434));
#8812=CARTESIAN_POINT('Ctrl Pts',(-1.53268946892128,-3.10797698807607,2.49925925223786));
#8813=CARTESIAN_POINT('Ctrl Pts',(1.7493988709872,-2.99136460950407,2.65639776575137));
#8814=CARTESIAN_POINT('Ctrl Pts',(3.46024629894863,-0.188026617557356,2.81353627926488));
#8815=CARTESIAN_POINT('Ctrl Pts',(2.06323722577413,2.78418938435949,2.97067479277839));
#8816=CARTESIAN_POINT('Ctrl Pts',(-1.18688998506621,3.25575653825361,3.12781330629191));
#8817=CARTESIAN_POINT('Ctrl Pts',(-3.3709995165217,0.803131807227777,3.28495181980542));
#8818=CARTESIAN_POINT('Ctrl Pts',(-2.52741049074122,-2.37083416635282,3.44209033331894));
#8819=CARTESIAN_POINT('Ctrl Pts',(0.586198762341201,-3.41541058398195,3.59922884683245));
#8820=CARTESIAN_POINT('Ctrl Pts',(3.17330745213002,-1.3924001776803,3.75636736034597));
#8821=CARTESIAN_POINT('Ctrl Pts',(2.91027678633445,1.88120904397026,3.91350587385948));
#8822=CARTESIAN_POINT('Ctrl Pts',(0.0333505152943699,3.46519064195013,4.07064438737299));
#8823=CARTESIAN_POINT('Ctrl Pts',(-2.87352987075533,1.93687493734171,4.22778290088651));
#8824=CARTESIAN_POINT('Ctrl Pts',(-3.19951927885268,-1.33106529716661,4.38492141440001));
#8825=CARTESIAN_POINT('Ctrl Pts',(-0.651826904677972,-3.40349528097662,
4.54205992791353));
#8826=CARTESIAN_POINT('Ctrl Pts',(2.48131063733581,-2.41904029776201,4.69919844142705));
#8827=CARTESIAN_POINT('Ctrl Pts',(3.38583301773356,0.738101088738959,4.85633695494055));
#8828=CARTESIAN_POINT('Ctrl Pts',(1.24933397805696,3.23230924456058,5.01347546845408));
#8829=CARTESIAN_POINT('Ctrl Pts',(-2.00926747133911,2.82338496663079,5.17061398196758));
#8830=CARTESIAN_POINT('Ctrl Pts',(-3.46322427730269,-0.12139211787978,5.3277524954811));
#8831=CARTESIAN_POINT('Ctrl Pts',(-1.80664989208085,-2.95713959911133,5.48489100899462));
#8832=CARTESIAN_POINT('Ctrl Pts',(1.47258603363221,-3.13690114838409,5.64202952250812));
#8833=CARTESIAN_POINT('Ctrl Pts',(3.4292033754596,-0.499222045701823,5.79916803602164));
#8834=CARTESIAN_POINT('Ctrl Pts',(2.30584575575073,2.58683857089803,5.95630654953515));
#8835=CARTESIAN_POINT('Ctrl Pts',(-0.888531402702859,3.34950300605675,6.11344506304867));
#8836=CARTESIAN_POINT('Ctrl Pts',(-3.28486476693535,1.10377620199891,6.27058357656218));
#8837=CARTESIAN_POINT('Ctrl Pts',(-2.73086240406331,-2.13331876928079,6.4277220900757));
#8838=CARTESIAN_POINT('Ctrl Pts',(0.275892655912234,-3.45435112336383,6.5848606035892));
#8839=CARTESIAN_POINT('Ctrl Pts',(3.03485183459055,-1.67282180255638,6.74199911710273));
#8840=CARTESIAN_POINT('Ctrl Pts',(3.06802702248421,1.6111699572782,6.89913763061623));
#8841=CARTESIAN_POINT('Ctrl Pts',(0.345621576330127,3.44807252913389,7.05627614412975));
#8842=CARTESIAN_POINT('Ctrl Pts',(-2.68720751132516,2.18805261171336,7.21341465764325));
#8843=CARTESIAN_POINT('Ctrl Pts',(-3.30649300260574,-1.03718969811004,7.37055317115678));
#8844=CARTESIAN_POINT('Ctrl Pts',(-0.956017138014702,-3.33086920560938,
7.52769168467029));
#8845=CARTESIAN_POINT('Ctrl Pts',(2.25311553735071,-2.63289362024357,7.68483019818381));
#8846=CARTESIAN_POINT('Ctrl Pts',(3.43858888024395,0.429842977951538,7.84196871169731));
#8847=CARTESIAN_POINT('Ctrl Pts',(1.53565755714059,3.10651158777771,7.99910722521083));
#8848=CARTESIAN_POINT('Ctrl Pts',(-1.74654067132524,2.99303427005181,8.15624573872433));
#8849=CARTESIAN_POINT('Ctrl Pts',(-3.46006514069016,0.191331803382343,8.31338425223787));
#8850=CARTESIAN_POINT('Ctrl Pts',(-2.06589572612039,-2.78221724805058,8.47052276575136));
#8851=CARTESIAN_POINT('Ctrl Pts',(1.183779392948,-3.25688886436581,8.62766127926489));
#8852=CARTESIAN_POINT('Ctrl Pts',(3.37023102179748,-0.806351310370959,8.7847997927784));
#8853=CARTESIAN_POINT('Ctrl Pts',(2.52967359714463,2.36841856552378,8.94193830629191));
#8854=CARTESIAN_POINT('Ctrl Pts',(-0.582935293544439,3.41596954985013,9.09907681980542));
#8855=CARTESIAN_POINT('Ctrl Pts',(-3.17197740603666,1.3954296219005,9.25621533331893));
#8856=CARTESIAN_POINT('Ctrl Pts',(-2.91206965945989,-1.87842613074489,9.41335384683245));
#8857=CARTESIAN_POINT('Ctrl Pts',(-0.0366657672894424,-3.46516125435096,
9.57049236034596));
#8858=CARTESIAN_POINT('Ctrl Pts',(2.8716885037831,-1.93961114588268,9.72763087385947));
#8859=CARTESIAN_POINT('Ctrl Pts',(3.20077001198978,1.32799366090119,9.88476938737299));
#8860=CARTESIAN_POINT('Ctrl Pts',(0.655114493273841,3.40289939669598,10.0419079008865));
#8861=CARTESIAN_POINT('Ctrl Pts',(-2.47906919875826,2.42135526672317,10.1990464144));
#8862=CARTESIAN_POINT('Ctrl Pts',(-3.3864019310671,-0.734763106864168,10.3561849279135));
#8863=CARTESIAN_POINT('Ctrl Pts',(-1.25267830620767,-3.23131219035953,10.513323441427));
#8864=CARTESIAN_POINT('Ctrl Pts',(2.00706204302524,-2.82492459714601,10.6704619549406));
#8865=CARTESIAN_POINT('Ctrl Pts',(3.46239353138226,0.117358798249391,10.8276004684541));
#8866=CARTESIAN_POINT('Ctrl Pts',(1.81131357477516,2.9568147670617,10.9847389819676));
#8867=CARTESIAN_POINT('Ctrl Pts',(-1.47339811761136,3.13548357068097,11.1418774954811));
#8868=CARTESIAN_POINT('Ctrl Pts',(-2.77050414434575,1.38461669033425,11.2466365044901));
#8869=CARTESIAN_POINT('Ctrl Pts',(-2.91090525077877,0.426608275808828,11.2990160089946));
#8870=CARTESIAN_POINT('Ctrl Pts',(1.59774743137964,-2.24059110187414,-0.219489327336925));
#8871=CARTESIAN_POINT('Ctrl Pts',(2.33514866714022,-1.71475623207252,-0.167109822832421));
#8872=CARTESIAN_POINT('Ctrl Pts',(3.23863136773739,0.11226788144075,-0.0623508138234118));
#8873=CARTESIAN_POINT('Ctrl Pts',(1.6876604910601,2.76982094937113,0.0947876996901019));
#8874=CARTESIAN_POINT('Ctrl Pts',(-1.38044412748324,2.93181193130462,0.251926213203615));
#8875=CARTESIAN_POINT('Ctrl Pts',(-3.2079816177237,0.464474356210045,0.409064726717129));
#8876=CARTESIAN_POINT('Ctrl Pts',(-2.15460694798876,-2.42206010021071,0.566203240230643));
#8877=CARTESIAN_POINT('Ctrl Pts',(0.834144210720117,-3.13213929648004,0.723341753744155));
#8878=CARTESIAN_POINT('Ctrl Pts',(3.07359869399491,-1.02960715343621,0.880480267257669));
#8879=CARTESIAN_POINT('Ctrl Pts',(2.55252127926951,1.99796636155783,1.03761878077118));
#8880=CARTESIAN_POINT('Ctrl Pts',(-0.261157599233816,3.2308943271893,1.19475729428469));
#8881=CARTESIAN_POINT('Ctrl Pts',(-2.84026054414775,1.56203972461538,1.35189580779821));
#8882=CARTESIAN_POINT('Ctrl Pts',(-2.86836128896387,-1.50981857631063,1.50903432131172));
#8883=CARTESIAN_POINT('Ctrl Pts',(-0.320209305227662,-3.22559586930712,
1.66617283482524));
#8884=CARTESIAN_POINT('Ctrl Pts',(2.51553994814305,-2.04428172839443,1.82331134833875));
#8885=CARTESIAN_POINT('Ctrl Pts',(3.09193171078347,0.973131394588079,1.98044986185226));
#8886=CARTESIAN_POINT('Ctrl Pts',(0.891272025644291,3.1165132590083,2.13758837536578));
#8887=CARTESIAN_POINT('Ctrl Pts',(-2.10989267602029,2.4607676867899,2.29472688887929));
#8888=CARTESIAN_POINT('Ctrl Pts',(-3.21603530707201,-0.405143027346019,
2.4518654023928));
#8889=CARTESIAN_POINT('Ctrl Pts',(-1.43366203071003,-2.90716984129947,2.60900391590632));
#8890=CARTESIAN_POINT('Ctrl Pts',(1.63636978576396,-2.79809181678146,2.76614242941983));
#8891=CARTESIAN_POINT('Ctrl Pts',(3.23667894658341,-0.175878172207005,2.92328094293335));
#8892=CARTESIAN_POINT('Ctrl Pts',(1.92993096835312,2.60430223316632,3.08041945644686));
#8893=CARTESIAN_POINT('Ctrl Pts',(-1.11020473535129,3.04540131890859,3.23755796996037));
#8894=CARTESIAN_POINT('Ctrl Pts',(-3.15319842040834,0.751241266431068,3.39469648347389));
#8895=CARTESIAN_POINT('Ctrl Pts',(-2.36411388612472,-2.21765399601942,3.5518349969874));
#8896=CARTESIAN_POINT('Ctrl Pts',(0.548324318173406,-3.19474007803184,3.70897351050091));
#8897=CARTESIAN_POINT('Ctrl Pts',(2.96827928823051,-1.30243686459143,3.86611202401443));
#8898=CARTESIAN_POINT('Ctrl Pts',(2.72224309752783,1.75966367151117,4.02325053752794));
#8899=CARTESIAN_POINT('Ctrl Pts',(0.0311957304148393,3.24130383438475,4.18038905104146));
#8900=CARTESIAN_POINT('Ctrl Pts',(-2.68787040907414,1.81173297801481,4.33752756455496));
#8901=CARTESIAN_POINT('Ctrl Pts',(-2.99279756247315,-1.24506484557935,4.49466607806848));
#8902=CARTESIAN_POINT('Ctrl Pts',(-0.609712210321215,-3.18359462564273,
4.65180459158199));
#8903=CARTESIAN_POINT('Ctrl Pts',(2.32099255542547,-2.26274551758992,4.80894310509551));
#8904=CARTESIAN_POINT('Ctrl Pts',(3.16707352551029,0.69041219843154,4.96608161860902));
#8905=CARTESIAN_POINT('Ctrl Pts',(1.16861420681437,3.02346896054623,5.12322013212254));
#8906=CARTESIAN_POINT('Ctrl Pts',(-1.87944821283798,2.64096537936348,5.28035864563605));
#8907=CARTESIAN_POINT('Ctrl Pts',(-3.23946451703395,-0.113548943710187,
5.43749715914956));
#8908=CARTESIAN_POINT('Ctrl Pts',(-1.68992180450333,-2.76607809260859,5.59463567266307));
#8909=CARTESIAN_POINT('Ctrl Pts',(1.37744189294803,-2.93422520459686,5.75177418617659));
#8910=CARTESIAN_POINT('Ctrl Pts',(3.20764171390784,-0.466967188284919,5.9089126996901));
#8911=CARTESIAN_POINT('Ctrl Pts',(2.15686450238375,2.41970230361335,6.06605121320362));
#8912=CARTESIAN_POINT('Ctrl Pts',(-0.831123173336083,3.13309080469669,6.22318972671712));
#8913=CARTESIAN_POINT('Ctrl Pts',(-3.07262885787747,1.03246095396017,6.38032824023064));
#8914=CARTESIAN_POINT('Ctrl Pts',(-2.55442072199701,-1.99548452634149,6.53746675374416));
#8915=CARTESIAN_POINT('Ctrl Pts',(0.258067164519323,-3.23116465972251,6.69460526725767));
#8916=CARTESIAN_POINT('Ctrl Pts',(2.83876932171097,-1.56474038029172,6.85174378077119));
#8917=CARTESIAN_POINT('Ctrl Pts',(2.86980105267096,1.50707187568543,7.00888229428469));
#8918=CARTESIAN_POINT('Ctrl Pts',(0.323290882482136,3.22529172698812,7.1660208077982));
#8919=CARTESIAN_POINT('Ctrl Pts',(-2.51358638246349,2.04668200194341,7.32315932131173));
#8920=CARTESIAN_POINT('Ctrl Pts',(-3.09285968799709,-0.970176620232505,
7.48029783482524));
#8921=CARTESIAN_POINT('Ctrl Pts',(-0.89424863892644,-3.11566093861428,7.63743634833875));
#8922=CARTESIAN_POINT('Ctrl Pts',(2.10754119617984,-2.46278172505391,7.79457486185227));
#8923=CARTESIAN_POINT('Ctrl Pts',(3.21642081895241,0.402070718924034,7.95171337536577));
#8924=CARTESIAN_POINT('Ctrl Pts',(1.43643835002984,2.90579912086969,8.1088518888793));
#8925=CARTESIAN_POINT('Ctrl Pts',(-1.63369625507517,2.79965360015637,8.2659904023928));
#8926=CARTESIAN_POINT('Ctrl Pts',(-3.23650949300394,0.178969809174445,8.42312891590632));
#8927=CARTESIAN_POINT('Ctrl Pts',(-1.93241770234741,-2.6024575170625,8.58026742941983));
#8928=CARTESIAN_POINT('Ctrl Pts',(1.10729511934404,-3.04646048515613,8.73740594293334));
#8929=CARTESIAN_POINT('Ctrl Pts',(3.15247957831459,-0.75425275669555,8.89454445644686));
#8930=CARTESIAN_POINT('Ctrl Pts',(2.36623077267467,2.21539446774564,9.05168296996036));
#8931=CARTESIAN_POINT('Ctrl Pts',(-0.54527170288688,3.19526292897974,9.20882148347389));
#8932=CARTESIAN_POINT('Ctrl Pts',(-2.96703517673773,1.30527057568604,9.36595999698739));
#8933=CARTESIAN_POINT('Ctrl Pts',(-2.72392013268591,-1.75706056298405,9.52309851050092));
#8934=CARTESIAN_POINT('Ctrl Pts',(-0.0342967831746755,-3.24127634552548,
9.68023702401442));
#8935=CARTESIAN_POINT('Ctrl Pts',(2.68614801326846,-1.81429239945851,9.83737553752795));
#8936=CARTESIAN_POINT('Ctrl Pts',(2.99396748543899,1.24219166847781,9.99451405104144));
#8937=CARTESIAN_POINT('Ctrl Pts',(0.612787387020777,3.18303724158995,10.151652564555));
#8938=CARTESIAN_POINT('Ctrl Pts',(-2.31889593673789,2.2649109158452,10.3087910780685));
#8939=CARTESIAN_POINT('Ctrl Pts',(-3.16760568121541,-0.687289884375024,
10.465929591582));
#8940=CARTESIAN_POINT('Ctrl Pts',(-1.17174245711238,-3.02253632625886,10.6230681050955));
#8941=CARTESIAN_POINT('Ctrl Pts',(1.8773852777822,-2.64240553397781,10.780206618609));
#8942=CARTESIAN_POINT('Ctrl Pts',(3.23868744580887,0.109776217839061,10.9373451321225));
#8943=CARTESIAN_POINT('Ctrl Pts',(1.69428416552798,2.76577424803644,11.0944836456361));
#8944=CARTESIAN_POINT('Ctrl Pts',(-1.37820150798437,2.93289921693286,11.2516221591496));
#8945=CARTESIAN_POINT('Ctrl Pts',(-2.59150119982806,1.29515627025004,11.3563811681586));
#8946=CARTESIAN_POINT('Ctrl Pts',(-2.72283095673203,0.399045011671044,11.4087606726631));
#8947=CARTESIAN_POINT('Ctrl Pts',(1.48738611075532,-2.08582659521589,-0.109744663668464));
#8948=CARTESIAN_POINT('Ctrl Pts',(2.17385277913045,-1.59631275433404,-0.0573651591639592));
#8949=CARTESIAN_POINT('Ctrl Pts',(3.01492915564857,0.104513194175331,0.0473938498450494));
#8950=CARTESIAN_POINT('Ctrl Pts',(1.57108859934498,2.57850091226017,0.204532363358563));
#8951=CARTESIAN_POINT('Ctrl Pts',(-1.28509261324199,2.72930267971312,0.361670876872076));
#8952=CARTESIAN_POINT('Ctrl Pts',(-2.98639647797178,0.432391686358259,0.51880939038559));
#8953=CARTESIAN_POINT('Ctrl Pts',(-2.00578163083517,-2.25476097267596,0.675947903899103));
#8954=CARTESIAN_POINT('Ctrl Pts',(0.776527309025778,-2.9157928187139,0.833086417412617));
#8955=CARTESIAN_POINT('Ctrl Pts',(2.86129579537873,-0.958489026161636,0.99022493092613));
#8956=CARTESIAN_POINT('Ctrl Pts',(2.37621079754423,1.85996069064019,1.14736344443964));
#8957=CARTESIAN_POINT('Ctrl Pts',(-0.243118642026661,3.00772653624605,1.30450195795316));
#8958=CARTESIAN_POINT('Ctrl Pts',(-2.64407502795598,1.45414484493007,1.46164047146667));
#8959=CARTESIAN_POINT('Ctrl Pts',(-2.67023476805036,-1.40553077167252,1.61877898498018));
#8960=CARTESIAN_POINT('Ctrl Pts',(-0.298091465381954,-3.00279405911757,
1.7759174984937));
#8961=CARTESIAN_POINT('Ctrl Pts',(2.34178388050189,-1.90307691288803,1.93305601200721));
#8962=CARTESIAN_POINT('Ctrl Pts',(2.87836249441012,0.905914221373807,2.09019452552073));
#8963=CARTESIAN_POINT('Ctrl Pts',(0.829709130374474,2.90124611962672,2.24733303903424));
#8964=CARTESIAN_POINT('Ctrl Pts',(-1.96415591091712,2.2907949074068,2.40447155254775));
#8965=CARTESIAN_POINT('Ctrl Pts',(-2.99389387426969,-0.37715855454295,2.56161006606126));
#8966=CARTESIAN_POINT('Ctrl Pts',(-1.33463459249878,-2.70636269452286,2.71874857957478));
#8967=CARTESIAN_POINT('Ctrl Pts',(1.52334070054072,-2.60481902405885,2.87588709308829));
#8968=CARTESIAN_POINT('Ctrl Pts',(3.01311159421818,-0.163729726856653,3.03302560660181));
#8969=CARTESIAN_POINT('Ctrl Pts',(1.79662471093212,2.42441508197314,3.19016412011532));
#8970=CARTESIAN_POINT('Ctrl Pts',(-1.03351948563637,2.83504609956357,3.34730263362884));
#8971=CARTESIAN_POINT('Ctrl Pts',(-2.93539732429499,0.699350725634357,3.50444114714234));
#8972=CARTESIAN_POINT('Ctrl Pts',(-2.20081728150821,-2.06447382568602,3.66157966065586));
#8973=CARTESIAN_POINT('Ctrl Pts',(0.510449874005612,-2.97406957208172,3.81871817416937));
#8974=CARTESIAN_POINT('Ctrl Pts',(2.763251124331,-1.21247355150257,3.97585668768289));
#8975=CARTESIAN_POINT('Ctrl Pts',(2.5342094087212,1.63811829905208,4.1329952011964));
#8976=CARTESIAN_POINT('Ctrl Pts',(0.029040945535309,3.01741702681936,4.29013371470992));
#8977=CARTESIAN_POINT('Ctrl Pts',(-2.50221094739296,1.68659101868791,4.44727222822342));
#8978=CARTESIAN_POINT('Ctrl Pts',(-2.78607584609361,-1.1590643939921,4.60441074173694));
#8979=CARTESIAN_POINT('Ctrl Pts',(-0.56759751596446,-2.96369397030884,4.76154925525046));
#8980=CARTESIAN_POINT('Ctrl Pts',(2.16067447351513,-2.10645073741783,4.91868776876396));
#8981=CARTESIAN_POINT('Ctrl Pts',(2.94831403328702,0.642723308124124,5.07582628227749));
#8982=CARTESIAN_POINT('Ctrl Pts',(1.08789443557179,2.81462867653188,5.23296479579099));
#8983=CARTESIAN_POINT('Ctrl Pts',(-1.74962895433684,2.45854579209617,5.39010330930451));
#8984=CARTESIAN_POINT('Ctrl Pts',(-3.01570475676522,-0.105705769540595,
5.54724182281802));
#8985=CARTESIAN_POINT('Ctrl Pts',(-1.57319371692581,-2.57501658610585,5.70438033633154));
#8986=CARTESIAN_POINT('Ctrl Pts',(1.28229775226384,-2.73154926080963,5.86151884984505));
#8987=CARTESIAN_POINT('Ctrl Pts',(2.98608005235609,-0.434712330868017,6.01865736335856));
#8988=CARTESIAN_POINT('Ctrl Pts',(2.00788324901678,2.25256603632868,6.17579587687208));
#8989=CARTESIAN_POINT('Ctrl Pts',(-0.773714943969305,2.91667860333663,6.33293439038559));
#8990=CARTESIAN_POINT('Ctrl Pts',(-2.86039294881959,0.961145705921419,6.4900729038991));
#8991=CARTESIAN_POINT('Ctrl Pts',(-2.37797903993071,-1.85765028340219,6.64721141741262));
#8992=CARTESIAN_POINT('Ctrl Pts',(0.240241673126412,-3.0079781960812,6.80434993092612));
#8993=CARTESIAN_POINT('Ctrl Pts',(2.64268680883139,-1.45665895802706,6.96148844443965));
#8994=CARTESIAN_POINT('Ctrl Pts',(2.67157508285772,1.40297379409266,7.11862695795316));
#8995=CARTESIAN_POINT('Ctrl Pts',(0.300960188634146,3.00251092484234,7.27576547146667));
#8996=CARTESIAN_POINT('Ctrl Pts',(-2.33996525360183,1.90531139217345,7.43290398498018));
#8997=CARTESIAN_POINT('Ctrl Pts',(-2.87922637338843,-0.903163542354968,
7.5900424984937));
#8998=CARTESIAN_POINT('Ctrl Pts',(-0.832480139838179,-2.90045267161919,
7.74718101200721));
#8999=CARTESIAN_POINT('Ctrl Pts',(1.96196685500896,-2.29266982986425,7.90431952552073));
#9000=CARTESIAN_POINT('Ctrl Pts',(2.99425275766087,0.37429845989653,8.06145803903424));
#9001=CARTESIAN_POINT('Ctrl Pts',(1.33721914291908,2.70508665396167,8.21859655254775));
#9002=CARTESIAN_POINT('Ctrl Pts',(-1.5208518388251,2.60627293026094,8.37573506606126));
#9003=CARTESIAN_POINT('Ctrl Pts',(-3.01295384531772,0.166607814966547,8.53287357957478));
#9004=CARTESIAN_POINT('Ctrl Pts',(-1.79893967857444,-2.42269778607442,8.69001209308829));
#9005=CARTESIAN_POINT('Ctrl Pts',(1.03081084574009,-2.83603210594645,8.8471506066018));
#9006=CARTESIAN_POINT('Ctrl Pts',(2.9347281348317,-0.702154203020143,9.00428912011532));
#9007=CARTESIAN_POINT('Ctrl Pts',(2.20278794820472,2.06237036996751,9.16142763362883));
#9008=CARTESIAN_POINT('Ctrl Pts',(-0.507608112229325,2.97455630810935,9.31856614714235));
#9009=CARTESIAN_POINT('Ctrl Pts',(-2.7620929474388,1.21511152947157,9.47570466065586));
#9010=CARTESIAN_POINT('Ctrl Pts',(-2.53577060591194,-1.63569499522321,9.63284317416937));
#9011=CARTESIAN_POINT('Ctrl Pts',(-0.0319277990599106,-3.0173914367,9.78998168768289));
#9012=CARTESIAN_POINT('Ctrl Pts',(2.50060752275382,-1.68897365303435,9.94712020119639));
#9013=CARTESIAN_POINT('Ctrl Pts',(2.78716495888821,1.15638967605443,10.1042587147099));
#9014=CARTESIAN_POINT('Ctrl Pts',(0.570460280767717,2.96317508648391,10.2613972282234));
#9015=CARTESIAN_POINT('Ctrl Pts',(-2.15872267471752,2.10846656496723,10.4185357417369));
#9016=CARTESIAN_POINT('Ctrl Pts',(-2.94880943136371,-0.639816661885883,
10.5756742552505));
#9017=CARTESIAN_POINT('Ctrl Pts',(-1.09080660801709,-2.8137604621582,10.732812768764));
#9018=CARTESIAN_POINT('Ctrl Pts',(1.74770851253917,-2.4598864708096,10.8899512822775));
#9019=CARTESIAN_POINT('Ctrl Pts',(3.01498136023548,0.102193637428725,11.047089795791));
#9020=CARTESIAN_POINT('Ctrl Pts',(1.57725475628079,2.57473372901119,11.2042283093045));
#9021=CARTESIAN_POINT('Ctrl Pts',(-1.28300489835739,2.73031486318474,11.361366822818));
#9022=CARTESIAN_POINT('Ctrl Pts',(-2.41249825531037,1.20569585016584,11.466125831827));
#9023=CARTESIAN_POINT('Ctrl Pts',(-2.53475666268528,0.371481747533259,11.5185053363315));
#9024=CARTESIAN_POINT('Ctrl Pts',(1.37702479013101,-1.93106208855765,-2.4980018054066E-15));
#9025=CARTESIAN_POINT('Ctrl Pts',(2.01255689112068,-1.47786927659557,0.052379504504502));
#9026=CARTESIAN_POINT('Ctrl Pts',(2.79122694355976,0.0967585069099138,0.157138513513511));
#9027=CARTESIAN_POINT('Ctrl Pts',(1.45451670762985,2.3871808751492,0.314277027027025));
#9028=CARTESIAN_POINT('Ctrl Pts',(-1.18974109900074,2.52679342812162,0.471415540540538));
#9029=CARTESIAN_POINT('Ctrl Pts',(-2.76481133821986,0.40030901650647,0.628554054054051));
#9030=CARTESIAN_POINT('Ctrl Pts',(-1.85695631368159,-2.0874618451412,0.785692567567565));
#9031=CARTESIAN_POINT('Ctrl Pts',(0.718910407331439,-2.69944634094777,0.942831081081078));
#9032=CARTESIAN_POINT('Ctrl Pts',(2.64899289676255,-0.887370898887054,1.09996959459459));
#9033=CARTESIAN_POINT('Ctrl Pts',(2.19990031581894,1.72195501972256,1.25710810810811));
#9034=CARTESIAN_POINT('Ctrl Pts',(-0.225079684819506,2.78455874530281,1.41424662162162));
#9035=CARTESIAN_POINT('Ctrl Pts',(-2.44788951176421,1.34624996524475,1.57138513513514));
#9036=CARTESIAN_POINT('Ctrl Pts',(-2.47210824713685,-1.30124296703442,1.72852364864864));
#9037=CARTESIAN_POINT('Ctrl Pts',(-0.275973625536248,-2.77999224892802,
1.88566216216216));
#9038=CARTESIAN_POINT('Ctrl Pts',(2.16802781286073,-1.76187209738162,2.04280067567567));
#9039=CARTESIAN_POINT('Ctrl Pts',(2.66479327803676,0.838697048159531,2.19993918918919));
#9040=CARTESIAN_POINT('Ctrl Pts',(0.76814623510466,2.68597898024514,2.3570777027027));
#9041=CARTESIAN_POINT('Ctrl Pts',(-1.81841914581395,2.1208221280237,2.51421621621621));
#9042=CARTESIAN_POINT('Ctrl Pts',(-2.77175244146736,-0.349174081739879,
2.67135472972972));
#9043=CARTESIAN_POINT('Ctrl Pts',(-1.23560715428754,-2.50555554774625,2.82849324324324));
#9044=CARTESIAN_POINT('Ctrl Pts',(1.41031161531747,-2.41154623133624,2.98563175675675));
#9045=CARTESIAN_POINT('Ctrl Pts',(2.78954424185296,-0.151581281506301,3.14277027027027));
#9046=CARTESIAN_POINT('Ctrl Pts',(1.66331845351111,2.24452793077997,3.29990878378378));
#9047=CARTESIAN_POINT('Ctrl Pts',(-0.956834235921451,2.62469088021855,3.45704729729729));
#9048=CARTESIAN_POINT('Ctrl Pts',(-2.71759622818163,0.647460184837647,3.61418581081081));
#9049=CARTESIAN_POINT('Ctrl Pts',(-2.03752067689171,-1.91129365535261,3.77132432432432));
#9050=CARTESIAN_POINT('Ctrl Pts',(0.47257542983782,-2.75339906613161,3.92846283783783));
#9051=CARTESIAN_POINT('Ctrl Pts',(2.55822296043148,-1.12251023841371,4.08560135135135));
#9052=CARTESIAN_POINT('Ctrl Pts',(2.34617571991457,1.51657292659299,4.24273986486486));
#9053=CARTESIAN_POINT('Ctrl Pts',(0.0268861606557786,2.79353021925399,4.39987837837838));
#9054=CARTESIAN_POINT('Ctrl Pts',(-2.31655148571177,1.56144905936101,4.55701689189189));
#9055=CARTESIAN_POINT('Ctrl Pts',(-2.57935412971408,-1.07306394240484,4.7141554054054));
#9056=CARTESIAN_POINT('Ctrl Pts',(-0.525482821607704,-2.74379331497496,
4.87129391891892));
#9057=CARTESIAN_POINT('Ctrl Pts',(2.00035639160479,-1.95015595724574,5.02843243243243));
#9058=CARTESIAN_POINT('Ctrl Pts',(2.72955454106374,0.595034417816705,5.18557094594594));
#9059=CARTESIAN_POINT('Ctrl Pts',(1.0071746643292,2.60578839251754,5.34270945945947));
#9060=CARTESIAN_POINT('Ctrl Pts',(-1.61980969583571,2.27612620482886,5.49984797297296));
#9061=CARTESIAN_POINT('Ctrl Pts',(-2.79194499649648,-0.0978625953710016,
5.6569864864865));
#9062=CARTESIAN_POINT('Ctrl Pts',(-1.45646562934828,-2.38395507960311,5.81412499999999));
#9063=CARTESIAN_POINT('Ctrl Pts',(1.18715361157964,-2.5288733170224,5.97126351351352));
#9064=CARTESIAN_POINT('Ctrl Pts',(2.76451839080433,-0.402457473451116,6.12840202702702));
#9065=CARTESIAN_POINT('Ctrl Pts',(1.8589019956498,2.08542976904401,6.28554054054054));
#9066=CARTESIAN_POINT('Ctrl Pts',(-0.716306714602523,2.70026640197657,6.44267905405405));
#9067=CARTESIAN_POINT('Ctrl Pts',(-2.64815703976171,0.889830457882673,6.59981756756756));
#9068=CARTESIAN_POINT('Ctrl Pts',(-2.20153735786441,-1.71981604046289,6.75695608108108));
#9069=CARTESIAN_POINT('Ctrl Pts',(0.222416181733502,-2.78479173243988,6.91409459459459));
#9070=CARTESIAN_POINT('Ctrl Pts',(2.4466042959518,-1.34857753576241,7.0712331081081));
#9071=CARTESIAN_POINT('Ctrl Pts',(2.47334911304448,1.29887571249989,7.22837162162162));
#9072=CARTESIAN_POINT('Ctrl Pts',(0.278629494786153,2.77973012269657,7.38551013513513));
#9073=CARTESIAN_POINT('Ctrl Pts',(-2.16634412474015,1.76394078240349,7.54264864864865));
#9074=CARTESIAN_POINT('Ctrl Pts',(-2.66559305877978,-0.83615046447743,7.69978716216215));
#9075=CARTESIAN_POINT('Ctrl Pts',(-0.770711640749916,-2.68524440462409,
7.85692567567567));
#9076=CARTESIAN_POINT('Ctrl Pts',(1.81639251383808,-2.12255793467458,8.01406418918919));
#9077=CARTESIAN_POINT('Ctrl Pts',(2.77208469636934,0.346526200869026,8.1712027027027));
#9078=CARTESIAN_POINT('Ctrl Pts',(1.23799993580832,2.50437418705365,8.32834121621622));
#9079=CARTESIAN_POINT('Ctrl Pts',(-1.40800742257503,2.4128922603655,8.48547972972973));
#9080=CARTESIAN_POINT('Ctrl Pts',(-2.78939819763151,0.154245820758651,8.64261824324324));
#9081=CARTESIAN_POINT('Ctrl Pts',(-1.66546165480147,-2.24293805508635,8.79975675675676));
#9082=CARTESIAN_POINT('Ctrl Pts',(0.954326572136137,-2.62560372673677,8.95689527027026));
#9083=CARTESIAN_POINT('Ctrl Pts',(2.71697669134881,-0.650055649344734,9.11403378378378));
#9084=CARTESIAN_POINT('Ctrl Pts',(2.03934512373477,1.90934627218937,9.2711722972973));
#9085=CARTESIAN_POINT('Ctrl Pts',(-0.469944521571767,2.75384968723896,9.42831081081079));
#9086=CARTESIAN_POINT('Ctrl Pts',(-2.55715071813987,1.12495248325711,9.58544932432433));
#9087=CARTESIAN_POINT('Ctrl Pts',(-2.34762107913798,-1.51432942746238,9.74258783783783));
#9088=CARTESIAN_POINT('Ctrl Pts',(-0.0295588149451427,-2.79350652787453,
9.89972635135136));
#9089=CARTESIAN_POINT('Ctrl Pts',(2.31506703223917,-1.56365490661018,10.0568648648649));
#9090=CARTESIAN_POINT('Ctrl Pts',(2.58036243233743,1.07058768363104,10.2140033783784));
#9091=CARTESIAN_POINT('Ctrl Pts',(0.528133174514654,2.74331293137788,10.3711418918919));
#9092=CARTESIAN_POINT('Ctrl Pts',(-1.99854941269714,1.95202221408926,10.5282804054054));
#9093=CARTESIAN_POINT('Ctrl Pts',(-2.73001318151202,-0.59234343939674,10.6854189189189));
#9094=CARTESIAN_POINT('Ctrl Pts',(-1.0098707589218,-2.60498459805753,10.8425574324324));
#9095=CARTESIAN_POINT('Ctrl Pts',(1.61803174729613,-2.2773674076414,10.999695945946));
#9096=CARTESIAN_POINT('Ctrl Pts',(2.79127527466209,0.0946110570183949,11.1568344594594));
#9097=CARTESIAN_POINT('Ctrl Pts',(1.46022534703361,2.38369320998594,11.313972972973));
#9098=CARTESIAN_POINT('Ctrl Pts',(-1.1878082887304,2.52773050943662,11.4711114864865));
#9099=CARTESIAN_POINT('Ctrl Pts',(-2.23349531079268,1.11623543008163,11.5758704954955));
#9100=CARTESIAN_POINT('Ctrl Pts',(-2.34668236863853,0.343918483395475,11.62825));
#9101=CARTESIAN_POINT('',(1.37702479013102,-1.93106208855765,0.));
#9102=CARTESIAN_POINT('Ctrl Pts',(1.37702479013101,-1.93106208855765,-2.4980018054066E-15));
#9103=CARTESIAN_POINT('Ctrl Pts',(2.01255689112068,-1.47786927659557,0.052379504504502));
#9104=CARTESIAN_POINT('Ctrl Pts',(2.79122694355976,0.0967585069099138,0.157138513513511));
#9105=CARTESIAN_POINT('Ctrl Pts',(1.45451670762985,2.3871808751492,0.314277027027025));
#9106=CARTESIAN_POINT('Ctrl Pts',(-1.18974109900074,2.52679342812162,0.471415540540538));
#9107=CARTESIAN_POINT('Ctrl Pts',(-2.31615344009055,1.00603694073732,0.583793234229858));
#9108=CARTESIAN_POINT('Ctrl Pts',(-2.37458477423974,0.11510370689526,0.643791423414673));
#9109=CARTESIAN_POINT('Ctrl Pts',(-2.37366757034868,0.001844716469488,0.651410108094984));
#9110=CARTESIAN_POINT('Ctrl Pts',(1.29197400994444,2.64783394680711,-2.46330733588707E-16));
#9111=CARTESIAN_POINT('Ctrl Pts',(1.37074936016223,2.60046826619745,-2.90204607120186E-16));
#9112=CARTESIAN_POINT('Ctrl Pts',(1.44700091320012,2.54930204226795,-5.92854700626308E-16));
#9113=CARTESIAN_POINT('Ctrl Pts',(1.5204041597113,2.49432533414619,-4.68375338513738E-16));
#9114=CARTESIAN_POINT('Ctrl Pts',(1.59876972116939,2.43563200920691,-3.1748808003354E-16));
#9115=CARTESIAN_POINT('Ctrl Pts',(1.67388955782072,2.37259497158855,9.42702435984343E-17));
#9116=CARTESIAN_POINT('Ctrl Pts',(1.74558455766593,2.30559334150577,2.91433543964104E-16));
#9117=CARTESIAN_POINT('Ctrl Pts',(1.78514524738377,2.26862241321206,4.00226572297347E-16));
#9118=CARTESIAN_POINT('Ctrl Pts',(1.82366240526687,2.23044382157621,2.41712413072573E-16));
#9119=CARTESIAN_POINT('Ctrl Pts',(1.86109995619813,2.19111823230724,2.56739074444567E-16));
#9120=CARTESIAN_POINT('Ctrl Pts',(1.87813922122651,2.17321964863167,2.63578284255041E-16));
#9121=CARTESIAN_POINT('Ctrl Pts',(1.89495840460327,2.15507923207588,-5.32738877742354E-17));
#9122=CARTESIAN_POINT('Ctrl Pts',(1.91153266312519,2.13672660521873,-9.0205620750794E-17));
#9123=CARTESIAN_POINT('Ctrl Pts',(1.97664662778045,2.0646261070319,-2.35296368099375E-16));
#9124=CARTESIAN_POINT('Ctrl Pts',(2.03804038590891,1.98919650283574,-3.72373475267393E-16));
#9125=CARTESIAN_POINT('Ctrl Pts',(2.09554796148623,1.91081666271006,-8.32667268468867E-17));
#9126=CARTESIAN_POINT('Ctrl Pts',(2.14343533270609,1.8455486617107,1.57476549926517E-16));
#9127=CARTESIAN_POINT('Ctrl Pts',(2.18862729734747,1.77823406218829,2.53857300975798E-16));
#9128=CARTESIAN_POINT('Ctrl Pts',(2.23100237945407,1.70908145885149,3.19189119579733E-16));
#9129=CARTESIAN_POINT('Ctrl Pts',(2.2495414778757,1.67882719489164,3.47771790218954E-16));
#9130=CARTESIAN_POINT('Ctrl Pts',(2.26754109313608,1.64822104628506,2.94521883274651E-16));
#9131=CARTESIAN_POINT('Ctrl Pts',(2.28498954152194,1.61728023964544,3.19189119579733E-16));
#9132=CARTESIAN_POINT('Ctrl Pts',(2.29543189661598,1.59876312668031,3.33951695310829E-16));
#9133=CARTESIAN_POINT('Ctrl Pts',(2.30567682494647,1.58012614919259,-6.61366324171955E-18));
#9134=CARTESIAN_POINT('Ctrl Pts',(2.31572165746038,1.56137299470242,-1.38777878078145E-17));
#9135=CARTESIAN_POINT('Ctrl Pts',(2.32292320728395,1.54792809393149,-1.90857347710862E-17));
#9136=CARTESIAN_POINT('Ctrl Pts',(2.33002152872364,1.53442403232929,-1.12870283643031E-16));
#9137=CARTESIAN_POINT('Ctrl Pts',(2.33700969851763,1.52087413145422,-1.11022302462516E-16));
#9138=CARTESIAN_POINT('Ctrl Pts',(2.38058260792534,1.43638725996736,-9.94996979838631E-17));
#9139=CARTESIAN_POINT('Ctrl Pts',(2.41994184512486,1.3499998824768,-3.77842799305168E-16));
#9140=CARTESIAN_POINT('Ctrl Pts',(2.45492973401008,1.26206183108408,-3.7470027081099E-16));
#9141=CARTESIAN_POINT('Ctrl Pts',(2.48961375478266,1.17488751738912,-3.71585035023886E-16));
#9142=CARTESIAN_POINT('Ctrl Pts',(2.52000223755862,1.08618841594484,-4.13121512185277E-16));
#9143=CARTESIAN_POINT('Ctrl Pts',(2.54589150534161,0.996296170221892,-3.7470027081099E-16));
#9144=CARTESIAN_POINT('Ctrl Pts',(2.57095558696702,0.909269120898709,-3.37503655671981E-16));
#9145=CARTESIAN_POINT('Ctrl Pts',(2.59180267862827,0.821123009321661,-1.98135956264892E-16));
#9146=CARTESIAN_POINT('Ctrl Pts',(2.60819974692058,0.732162501184589,-2.77555756156289E-16));
#9147=CARTESIAN_POINT('Ctrl Pts',(2.61796168819389,0.679200152025794,-3.24838075693952E-16));
#9148=CARTESIAN_POINT('Ctrl Pts',(2.62614545111416,0.625949276096869,-2.51374357035676E-17));
#9149=CARTESIAN_POINT('Ctrl Pts',(2.63269335080009,0.572476447093945,0.));
#9150=CARTESIAN_POINT('Ctrl Pts',(2.6352683765624,0.5514477327168,9.88554309620052E-18));
#9151=CARTESIAN_POINT('Ctrl Pts',(2.63759088070415,0.530377846603737,-5.43523939458827E-17));
#9152=CARTESIAN_POINT('Ctrl Pts',(2.63965388200594,0.50930758122065,-2.77555756156289E-17));
#9153=CARTESIAN_POINT('Ctrl Pts',(2.64834931960739,0.420497565576959,8.43485582923526E-17));
#9154=CARTESIAN_POINT('Ctrl Pts',(2.65245297898025,0.3315870178655,7.13394232030532E-17));
#9155=CARTESIAN_POINT('Ctrl Pts',(2.65178792227632,0.242870082265014,1.11022302462516E-16));
#9156=CARTESIAN_POINT('Ctrl Pts',(2.65141677862428,0.193360428001277,1.33167855834344E-16));
#9157=CARTESIAN_POINT('Ctrl Pts',(2.64955959473733,0.143911103160085,2.55410202784461E-16));
#9158=CARTESIAN_POINT('Ctrl Pts',(2.64617859082989,0.0945743399740305,2.77555756156289E-16));
#9159=CARTESIAN_POINT('Ctrl Pts',(2.63998980161557,0.00426541509996067,
2.91350122435194E-16));
#9160=CARTESIAN_POINT('Ctrl Pts',(2.62869784498548,-0.0856678806083358,
1.22336690906674E-16));
#9161=CARTESIAN_POINT('Ctrl Pts',(2.61249699286393,-0.174890907412304,1.94289029309402E-16));
#9162=CARTESIAN_POINT('Ctrl Pts',(2.59606370990205,-0.265394001643718,2.67273655542046E-16));
#9163=CARTESIAN_POINT('Ctrl Pts',(2.57457910556097,-0.355167245076682,-8.63540186836622E-17));
#9164=CARTESIAN_POINT('Ctrl Pts',(2.54820206281091,-0.443829678011398,-1.94289029309402E-16));
#9165=CARTESIAN_POINT('Ctrl Pts',(2.5433159398537,-0.460253640057088,-2.14283072550056E-16));
#9166=CARTESIAN_POINT('Ctrl Pts',(2.53826078384047,-0.476642310793062,2.54370247567095E-16));
#9167=CARTESIAN_POINT('Ctrl Pts',(2.53304532831965,-0.49296952041645,2.4980018054066E-16));
#9168=CARTESIAN_POINT('Ctrl Pts',(2.5060606614482,-0.577446189974434,2.26154741365496E-16));
#9169=CARTESIAN_POINT('Ctrl Pts',(2.47475215402615,-0.660408357948197,3.47506847049484E-16));
#9170=CARTESIAN_POINT('Ctrl Pts',(2.43933604293942,-0.741555503604727,2.77555756156289E-16));
#9171=CARTESIAN_POINT('Ctrl Pts',(2.40393876465244,-0.822659498618874,2.07641862313994E-16));
#9172=CARTESIAN_POINT('Ctrl Pts',(2.3644375894048,-0.901951185787608,-1.23823437954767E-16));
#9173=CARTESIAN_POINT('Ctrl Pts',(2.32100582430644,-0.979100944080977,-1.11022302462516E-16));
#9174=CARTESIAN_POINT('Ctrl Pts',(2.27823644108386,-1.05507408425856,-9.84163982743666E-17));
#9175=CARTESIAN_POINT('Ctrl Pts',(2.23165476456022,-1.1289707546069,2.53313632717541E-16));
#9176=CARTESIAN_POINT('Ctrl Pts',(2.18139506127574,-1.20043719637909,2.77555756156289E-16));
#9177=CARTESIAN_POINT('Ctrl Pts',(2.16608689289344,-1.2222045418435,2.84939454890925E-16));
#9178=CARTESIAN_POINT('Ctrl Pts',(2.15043733121093,-1.24374612322857,4.37114965090439E-17));
#9179=CARTESIAN_POINT('Ctrl Pts',(2.13444972694369,-1.26505107698559,0.));
#9180=CARTESIAN_POINT('Ctrl Pts',(2.12083931058568,-1.28318820912085,-3.72120586158607E-17));
#9181=CARTESIAN_POINT('Ctrl Pts',(2.10698390104784,-1.30115384375424,6.4814165885223E-17));
#9182=CARTESIAN_POINT('Ctrl Pts',(2.09288546869145,-1.31894102140198,5.55111512312578E-17));
#9183=CARTESIAN_POINT('Ctrl Pts',(2.08472665052523,-1.32923453095322,5.01274601200272E-17));
#9184=CARTESIAN_POINT('Ctrl Pts',(2.07648733901943,-1.33946704131009,1.07093663002969E-16));
#9185=CARTESIAN_POINT('Ctrl Pts',(2.06817568052718,-1.3496280615777,1.11022302462516E-16));
#9186=CARTESIAN_POINT('Ctrl Pts',(2.0141423836499,-1.41568388247163,1.36562011828508E-16));
#9187=CARTESIAN_POINT('Ctrl Pts',(1.95696807639868,-1.47883106712894,-2.06909962337776E-16));
#9188=CARTESIAN_POINT('Ctrl Pts',(1.89681447147471,-1.5387754276769,-2.22044604925031E-16));
#9189=CARTESIAN_POINT('Ctrl Pts',(1.83758356202805,-1.5978003023447,-2.36947097397864E-16));
#9190=CARTESIAN_POINT('Ctrl Pts',(1.77546340770889,-1.65372037608364,4.0590157288843E-16));
#9191=CARTESIAN_POINT('Ctrl Pts',(1.71058212140457,-1.70621256947127,4.44089209850063E-16));
#9192=CARTESIAN_POINT('Ctrl Pts',(1.64772546517897,-1.75706673624623,4.81085195985522E-16));
#9193=CARTESIAN_POINT('Ctrl Pts',(1.58227673616169,-1.80470390837557,2.58606592525932E-16));
#9194=CARTESIAN_POINT('Ctrl Pts',(1.5143365021986,-1.84878472647799,2.77555756156289E-16));
#9195=CARTESIAN_POINT('Ctrl Pts',(1.46963595841736,-1.87778722506477,2.90023153883192E-16));
#9196=CARTESIAN_POINT('Ctrl Pts',(1.42385657678108,-1.90524929950103,3.23574125955808E-17));
#9197=CARTESIAN_POINT('Ctrl Pts',(1.37702479013104,-1.93106208855763,5.55111512312578E-17));
#9198=CARTESIAN_POINT('Ctrl Pts',(0.261124777554701,2.92529416030267,11.058));
#9199=CARTESIAN_POINT('Ctrl Pts',(0.712806568001128,2.88599464153458,11.0335796606559));
#9200=CARTESIAN_POINT('Ctrl Pts',(1.15551467718148,2.74786827548953,11.0091593213117));
#9201=CARTESIAN_POINT('Ctrl Pts',(1.53904161881194,2.51335023952951,10.9847389819676));
#9202=CARTESIAN_POINT('Ctrl Pts',(2.36167356031087,2.01032944412425,10.9323594774631));
#9203=CARTESIAN_POINT('Ctrl Pts',(2.91203354584656,1.06384412118684,10.8799799729586));
#9204=CARTESIAN_POINT('Ctrl Pts',(2.94465829055491,0.100220893818898,10.8276004684541));
#9205=CARTESIAN_POINT('Ctrl Pts',(2.97728303526326,-0.863402333549067,10.7752209639496));
#9206=CARTESIAN_POINT('Ctrl Pts',(2.49217253914424,-1.84416346534755,10.7228414594451));
#9207=CARTESIAN_POINT('Ctrl Pts',(1.70632723287924,-2.40227529678238,10.6704619549406));
#9208=CARTESIAN_POINT('Ctrl Pts',(0.92048192661426,-2.96038712821718,10.6180824504361));
#9209=CARTESIAN_POINT('Ctrl Pts',(-0.166098189796688,-3.09584965928835,
10.5657029459315));
#9210=CARTESIAN_POINT('Ctrl Pts',(-1.0650088521454,-2.74748941090806,10.513323441427));
#9211=CARTESIAN_POINT('Ctrl Pts',(-1.96391951449414,-2.39912916252775,10.4609439369225));
#9212=CARTESIAN_POINT('Ctrl Pts',(-2.67516072278063,-1.56694613469595,10.408564432418));
#9213=CARTESIAN_POINT('Ctrl Pts',(-2.87955920487239,-0.624834891848815,
10.3561849279135));
#9214=CARTESIAN_POINT('Ctrl Pts',(-2.92379628688831,-0.420937818389941,
10.3448486576389));
#9215=CARTESIAN_POINT('Ctrl Pts',(-2.94429281596354,-0.211891698741057,
10.3335123873642));
#9216=CARTESIAN_POINT('Ctrl Pts',(-2.94242444587263,-0.00248500551853048,
10.3221761170896));
#9217=CARTESIAN_POINT('Origin',(0.,0.,-1.84858989190501));
#9218=CARTESIAN_POINT('',(-1.37702479013099,-1.93106208855767,0.));
#9219=CARTESIAN_POINT('Ctrl Pts',(-1.37989654081094,-1.93326688769301,3.07371315899641E-16));
#9220=CARTESIAN_POINT('Ctrl Pts',(-0.801986922861967,-2.34019513141193,
0.0475906520026623));
#9221=CARTESIAN_POINT('Ctrl Pts',(0.824868299691477,-2.62988338064349,0.147626409229032));
#9222=CARTESIAN_POINT('Ctrl Pts',(2.66596861578497,-0.838738147770652,0.30010727167911));
#9223=CARTESIAN_POINT('Ctrl Pts',(2.16631806184957,1.76615982799916,0.457442587350233));
#9224=CARTESIAN_POINT('Ctrl Pts',(-0.283824062622952,2.78024166545816,0.614777903021357));
#9225=CARTESIAN_POINT('Ctrl Pts',(-2.10236314538525,1.54689613835291,0.745160337872953));
#9226=CARTESIAN_POINT('Ctrl Pts',(-2.3682722008076,0.381486792202907,0.823097667500842));
#9227=CARTESIAN_POINT('Ctrl Pts',(-2.36802324146013,0.000186122305323062,
0.848589891905023));
#9228=CARTESIAN_POINT('Origin',(0.,0.,0.));
#9229=CARTESIAN_POINT('Ctrl Pts',(-1.03908919352509,2.13201587949044,-0.329233991005384));
#9230=CARTESIAN_POINT('Ctrl Pts',(-1.74163600084562,1.78961280339009,-0.276788885781676));
#9231=CARTESIAN_POINT('Ctrl Pts',(-2.77044124913769,0.362429281341372,-0.171898675334261));
#9232=CARTESIAN_POINT('Ctrl Pts',(-1.82442757362648,-2.1194917921021,-0.0145633596631371));
#9233=CARTESIAN_POINT('Ctrl Pts',(0.766254154833431,-2.68690713172521,0.142771956007986));
#9234=CARTESIAN_POINT('Ctrl Pts',(2.66596861578497,-0.838738147770652,0.30010727167911));
#9235=CARTESIAN_POINT('Ctrl Pts',(2.16631806184957,1.76615982799916,0.457442587350233));
#9236=CARTESIAN_POINT('Ctrl Pts',(-0.283824062622952,2.78024166545816,0.614777903021357));
#9237=CARTESIAN_POINT('Ctrl Pts',(-2.47829466728951,1.29193683314281,0.772113218692479));
#9238=CARTESIAN_POINT('Ctrl Pts',(-2.44182858239548,-1.35964121596809,0.929448534363604));
#9239=CARTESIAN_POINT('Ctrl Pts',(-0.207121339063888,-2.78711087979173,
1.08678385003473));
#9240=CARTESIAN_POINT('Ctrl Pts',(2.21401803077907,-1.70561830406782,1.24411916570585));
#9241=CARTESIAN_POINT('Ctrl Pts',(2.64205485235054,0.911349150745493,1.40145448137697));
#9242=CARTESIAN_POINT('Ctrl Pts',(0.691640660298454,2.70787919402874,1.5587897970481));
#9243=CARTESIAN_POINT('Ctrl Pts',(-1.88140253096646,2.06671733364312,1.71612511271922));
#9244=CARTESIAN_POINT('Ctrl Pts',(-2.76076141176456,-0.43496057134077,1.87346042839035));
#9245=CARTESIAN_POINT('Ctrl Pts',(-1.15481219883121,-2.54507342378116,2.03079574406147));
#9246=CARTESIAN_POINT('Ctrl Pts',(1.49072764255621,-2.36404822464922,2.18813105973259));
#9247=CARTESIAN_POINT('Ctrl Pts',(2.79427705549031,-0.0548463935276453,
2.34546637540372));
#9248=CARTESIAN_POINT('Ctrl Pts',(1.5823475414007,2.30372918060613,2.50280169107483));
#9249=CARTESIAN_POINT('Ctrl Pts',(-1.05405113312049,2.58842974112365,2.66013700674597));
#9250=CARTESIAN_POINT('Ctrl Pts',(-2.74156638658485,0.542960359863138,2.81747232241708));
#9251=CARTESIAN_POINT('Ctrl Pts',(-1.9610543025963,-1.99129560121778,2.97480763808821));
#9252=CARTESIAN_POINT('Ctrl Pts',(0.584848394656438,-2.73293698550247,3.13214295375933));
#9253=CARTESIAN_POINT('Ctrl Pts',(2.60425579784155,-1.01431944186932,3.28947826943046));
#9254=CARTESIAN_POINT('Ctrl Pts',(2.27924634057658,1.61741407950708,3.44681358510158));
#9255=CARTESIAN_POINT('Ctrl Pts',(-0.0975982492034651,2.79311059143494,
3.6041489007727));
#9256=CARTESIAN_POINT('Ctrl Pts',(-2.38658243027454,1.45437838755459,3.76148421644382));
#9257=CARTESIAN_POINT('Ctrl Pts',(-2.52710481755741,-1.19362198012869,3.91881953211495));
#9258=CARTESIAN_POINT('Ctrl Pts',(-0.392663608746353,-2.76709368867159,
4.07615484778607));
#9259=CARTESIAN_POINT('Ctrl Pts',(2.09526330020315,-1.8495577562663,4.23349016345719));
#9260=CARTESIAN_POINT('Ctrl Pts',(2.69698125586998,0.732996791565816,4.39082547912832));
#9261=CARTESIAN_POINT('Ctrl Pts',(0.870808554093777,2.65568911080063,4.54816079479944));
#9262=CARTESIAN_POINT('Ctrl Pts',(-1.73928800639316,2.18766300463189,4.70549611047057));
#9263=CARTESIAN_POINT('Ctrl Pts',(-2.78363356575401,-0.249752602863106,
4.86283142614169));
#9264=CARTESIAN_POINT('Ctrl Pts',(-1.32208186928512,-2.46233460804071,5.02016674181281));
#9265=CARTESIAN_POINT('Ctrl Pts',(1.32964132424929,-2.45826079574207,5.17750205748394));
#9266=CARTESIAN_POINT('Ctrl Pts',(2.78438780839412,-0.241198514719961,5.33483737315506));
#9267=CARTESIAN_POINT('Ctrl Pts',(1.73255804842731,2.19299676239354,5.49217268882618));
#9268=CARTESIAN_POINT('Ctrl Pts',(-0.878964234485193,2.65300095467984,5.64950800449731));
#9269=CARTESIAN_POINT('Ctrl Pts',(-2.69922070918587,0.72470666765315,5.80684332016843));
#9270=CARTESIAN_POINT('Ctrl Pts',(-2.08957051396587,-1.85598686908106,5.96417863583956));
#9271=CARTESIAN_POINT('Ctrl Pts',(0.401163844498212,-2.76587414046649,6.12151395151068));
#9272=CARTESIAN_POINT('Ctrl Pts',(2.53076037597685,-1.18585163930103,6.2788492671818));
#9273=CARTESIAN_POINT('Ctrl Pts',(2.38210248511723,1.46170446446183,6.43618458285292));
#9274=CARTESIAN_POINT('Ctrl Pts',(0.0890157606711408,2.793397283841,6.59351989852405));
#9275=CARTESIAN_POINT('Ctrl Pts',(-2.28420520026003,1.61040330172691,6.75085521419516));
#9276=CARTESIAN_POINT('Ctrl Pts',(-2.60112693645964,-1.02231641451357,6.9081905298663));
#9277=CARTESIAN_POINT('Ctrl Pts',(-0.57644849505612,-2.73472106868152,7.06552584553741));
#9278=CARTESIAN_POINT('Ctrl Pts',(1.96716344393165,-1.98526073259378,7.22286116120855));
#9279=CARTESIAN_POINT('Ctrl Pts',(2.73988515609665,0.551381466653972,7.38019647687966));
#9280=CARTESIAN_POINT('Ctrl Pts',(1.04609303646807,2.5916561403346,7.53753179255079));
#9281=CARTESIAN_POINT('Ctrl Pts',(-1.58941846186445,2.2988564868904,7.69486710822191));
#9282=CARTESIAN_POINT('Ctrl Pts',(-2.79409530723714,-0.0634318507917163,
7.85220242389303));
#9283=CARTESIAN_POINT('Ctrl Pts',(-1.48345697628832,-2.36861723168749,8.00953773956416));
#9284=CARTESIAN_POINT('Ctrl Pts',(1.16262680634646,-2.54151354917186,8.16687305523529));
#9285=CARTESIAN_POINT('Ctrl Pts',(2.76208455499713,-0.426475157784177,8.3242083709064));
#9286=CARTESIAN_POINT('Ctrl Pts',(1.8750440359881,2.07248692819523,8.48154368657753));
#9287=CARTESIAN_POINT('Ctrl Pts',(-0.699958537943023,2.7057439570526,8.63887900224866));
#9288=CARTESIAN_POINT('Ctrl Pts',(-2.6448406647993,0.903221864868725,8.79621431791976));
#9289=CARTESIAN_POINT('Ctrl Pts',(-2.20877058145475,-1.7124032551425,8.95354963359091));
#9290=CARTESIAN_POINT('Ctrl Pts',(0.215690902196592,-2.78647992051942,9.11088494926201));
#9291=CARTESIAN_POINT('Ctrl Pts',(2.4459813653409,-1.35209655994371,9.26822026493315));
#9292=CARTESIAN_POINT('Ctrl Pts',(2.47433880171217,1.29947749716991,9.42555558060427));
#9293=CARTESIAN_POINT('Ctrl Pts',(0.275231669725872,2.78123058171878,9.58289089627539));
#9294=CARTESIAN_POINT('Ctrl Pts',(-2.17164161907558,1.7592467736877,9.74022621194653));
#9295=CARTESIAN_POINT('Ctrl Pts',(-2.66355657074516,-0.846449946443288,
9.89756152761763));
#9296=CARTESIAN_POINT('Ctrl Pts',(-0.757654725048104,-2.69016151139635,
10.0548968432888));
#9297=CARTESIAN_POINT('Ctrl Pts',(1.83027666927001,-2.11210170665972,10.2122321589599));
#9298=CARTESIAN_POINT('Ctrl Pts',(2.77060484795253,0.367287133540841,10.369567474631));
#9299=CARTESIAN_POINT('Ctrl Pts',(1.21665350181368,2.51610800548609,10.5269027903021));
#9300=CARTESIAN_POINT('Ctrl Pts',(-1.43234772356642,2.39972494583597,10.6842381059733));
#9301=CARTESIAN_POINT('Ctrl Pts',(-2.79231938150401,0.123316482315984,10.8415734216444));
#9302=CARTESIAN_POINT('Ctrl Pts',(-1.63779792657952,-2.26461658842463,10.9989087373155));
#9303=CARTESIAN_POINT('Ctrl Pts',(0.989622905930635,-2.61290295808564,11.1562440529866));
#9304=CARTESIAN_POINT('Ctrl Pts',(2.72902843688469,-0.61088887604173,11.3135793686578));
#9305=CARTESIAN_POINT('Ctrl Pts',(2.00599839187704,1.9449087769569,11.4709146843289));
#9306=CARTESIAN_POINT('Ctrl Pts',(0.328567026486064,2.47549058867235,11.5758048947763));
#9307=CARTESIAN_POINT('Ctrl Pts',(-0.439445221994061,2.3306835819919,11.62825));
#9308=CARTESIAN_POINT('Ctrl Pts',(-1.12236674703447,2.30288577939268,-0.219489327336923));
#9309=CARTESIAN_POINT('Ctrl Pts',(-1.881218999262,1.93304089110777,-0.167044222113215));
#9310=CARTESIAN_POINT('Ctrl Pts',(-2.9924775967461,0.391476088928602,-0.0621540116657994));
#9311=CARTESIAN_POINT('Ctrl Pts',(-1.97064588273166,-2.28935795203269,0.0951813040053245));
#9312=CARTESIAN_POINT('Ctrl Pts',(0.82766540978493,-2.90224865758394,0.252516619676447));
#9313=CARTESIAN_POINT('Ctrl Pts',(2.87963202931947,-0.905958614903406,0.409851935347572));
#9314=CARTESIAN_POINT('Ctrl Pts',(2.33993710190716,1.90770828264466,0.567187251018694));
#9315=CARTESIAN_POINT('Ctrl Pts',(-0.306571073860874,3.00306346507554,0.724522566689817));
#9316=CARTESIAN_POINT('Ctrl Pts',(-2.67691699735827,1.39547879991837,0.881857882360941));
#9317=CARTESIAN_POINT('Ctrl Pts',(-2.63752834686069,-1.46860933422193,1.03919319803207));
#9318=CARTESIAN_POINT('Ctrl Pts',(-0.223721028969555,-3.01048321093979,
1.19652851370319));
#9319=CARTESIAN_POINT('Ctrl Pts',(2.39145997337443,-1.84231467283839,1.35386382937431));
#9320=CARTESIAN_POINT('Ctrl Pts',(2.85380170306596,0.984389009248359,1.51119914504543));
#9321=CARTESIAN_POINT('Ctrl Pts',(0.747072034675363,2.92490152077689,1.66853446071656));
#9322=CARTESIAN_POINT('Ctrl Pts',(-2.03218708432488,2.23235389729304,1.82586977638768));
#9323=CARTESIAN_POINT('Ctrl Pts',(-2.98202197113476,-0.469820381720866,
1.98320509205881));
#9324=CARTESIAN_POINT('Ctrl Pts',(-1.24736434476896,-2.74904772122835,2.14054040772993));
#9325=CARTESIAN_POINT('Ctrl Pts',(1.61020165094208,-2.55351430104939,2.29787572340105));
#9326=CARTESIAN_POINT('Ctrl Pts',(3.01822371806624,-0.0592420445461263,
2.45521103907218));
#9327=CARTESIAN_POINT('Ctrl Pts',(1.70916440454448,2.48836100172844,2.6125463547433));
#9328=CARTESIAN_POINT('Ctrl Pts',(-1.13852780768032,2.79587882019688,2.76988167041443));
#9329=CARTESIAN_POINT('Ctrl Pts',(-2.9612885652785,0.586475787319947,2.92721698608554));
#9330=CARTESIAN_POINT('Ctrl Pts',(-2.11822252803541,-2.15088750826171,3.08455230175667));
#9331=CARTESIAN_POINT('Ctrl Pts',(0.631720928587459,-2.95196756292179,3.24188761742779));
#9332=CARTESIAN_POINT('Ctrl Pts',(2.81297325242419,-1.09561182958951,3.39922293309892));
#9333=CARTESIAN_POINT('Ctrl Pts',(2.46191599037299,1.74704134191371,3.55655824877004));
#9334=CARTESIAN_POINT('Ctrl Pts',(-0.105420237413036,3.01696376802969,3.71389356444116));
#9335=CARTESIAN_POINT('Ctrl Pts',(-2.57785450516496,1.57093919364055,3.87122888011228));
#9336=CARTESIAN_POINT('Ctrl Pts',(-2.72963902538035,-1.28928452665457,4.02856419578341));
#9337=CARTESIAN_POINT('Ctrl Pts',(-0.424133539231963,-2.98886174685155,
4.18589951145453));
#9338=CARTESIAN_POINT('Ctrl Pts',(2.26318767347756,-1.99779011781522,4.34323482712566));
#9339=CARTESIAN_POINT('Ctrl Pts',(2.91313016998542,0.791742643136777,4.50057014279678));
#9340=CARTESIAN_POINT('Ctrl Pts',(0.940599296228219,2.86852867588043,4.6579054584679));
#9341=CARTESIAN_POINT('Ctrl Pts',(-1.87868282535885,2.36299272999521,4.81524077413902));
#9342=CARTESIAN_POINT('Ctrl Pts',(-3.00672720840483,-0.269768965152914,
4.97257608981016));
#9343=CARTESIAN_POINT('Ctrl Pts',(-1.42803980273229,-2.65967782299944,5.12991140548127));
#9344=CARTESIAN_POINT('Ctrl Pts',(1.43620510839645,-2.65527751599392,5.28724672115241));
#9345=CARTESIAN_POINT('Ctrl Pts',(3.00754189963992,-0.260529311672868,5.44458203682351));
#9346=CARTESIAN_POINT('Ctrl Pts',(1.87141349653044,2.36875396048986,5.60191735249465));
#9347=CARTESIAN_POINT('Ctrl Pts',(-0.949408611663097,2.86562507813386,5.75925266816576));
#9348=CARTESIAN_POINT('Ctrl Pts',(-2.9155491037487,0.782788109236974,5.9165879838369));
#9349=CARTESIAN_POINT('Ctrl Pts',(-2.25703864025646,-2.00473449033026,6.07392329950801));
#9350=CARTESIAN_POINT('Ctrl Pts',(0.433315024333776,-2.98754445824887,6.23125861517914));
#9351=CARTESIAN_POINT('Ctrl Pts',(2.73358755765012,-1.28089143373012,6.38859393085026));
#9352=CARTESIAN_POINT('Ctrl Pts',(2.57301551588047,1.57885241721953,6.54592924652138));
#9353=CARTESIAN_POINT('Ctrl Pts',(0.0961499074014511,3.01727343732968,6.70326456219251));
#9354=CARTESIAN_POINT('Ctrl Pts',(-2.46727227667312,1.73946868703451,6.86059987786364));
#9355=CARTESIAN_POINT('Ctrl Pts',(-2.80959362919934,-1.104249717683,7.01793519353475));
#9356=CARTESIAN_POINT('Ctrl Pts',(-0.622647821053927,-2.95389463101813,
7.17527050920589));
#9357=CARTESIAN_POINT('Ctrl Pts',(2.12482128503379,-2.14436897654329,7.33260582487699));
#9358=CARTESIAN_POINT('Ctrl Pts',(2.95947259297716,0.59557180168919,7.48994114054813));
#9359=CARTESIAN_POINT('Ctrl Pts',(1.12993191128569,2.79936379839662,7.64727645621924));
#9360=CARTESIAN_POINT('Ctrl Pts',(-1.71680202222819,2.4830977871468,7.80461177189038));
#9361=CARTESIAN_POINT('Ctrl Pts',(-3.01802740364303,-0.0685155812177535,
7.96194708756148));
#9362=CARTESIAN_POINT('Ctrl Pts',(-1.60234827887482,-2.55844949005786,8.11928240323263));
#9363=CARTESIAN_POINT('Ctrl Pts',(1.25580525212405,-2.74520254132467,8.27661771890373));
#9364=CARTESIAN_POINT('Ctrl Pts',(2.98345115736347,-0.460654906735591,8.43395303457487));
#9365=CARTESIAN_POINT('Ctrl Pts',(2.02531898929576,2.23858589461288,8.591288350246));
#9366=CARTESIAN_POINT('Ctrl Pts',(-0.756056546623237,2.92259515574686,8.74862366591711));
#9367=CARTESIAN_POINT('Ctrl Pts',(-2.85681078378342,0.975610363999675,8.90595898158824));
#9368=CARTESIAN_POINT('Ctrl Pts',(-2.38579196848608,-1.84964340218511,9.06329429725935));
#9369=CARTESIAN_POINT('Ctrl Pts',(0.232977397678477,-3.00980168358836,9.2206296129305));
#9370=CARTESIAN_POINT('Ctrl Pts',(2.6420139535965,-1.46046001355504,9.37796492860159));
#9371=CARTESIAN_POINT('Ctrl Pts',(2.67264408988566,1.40362380865033,9.53530024427275));
#9372=CARTESIAN_POINT('Ctrl Pts',(0.297290045701602,3.00413163779202,9.69263555994384));
#9373=CARTESIAN_POINT('Ctrl Pts',(-2.34568731434669,1.90024118325806,9.84997087561499));
#9374=CARTESIAN_POINT('Ctrl Pts',(-2.87702667151006,-0.914288473825907,
10.0073061912861));
#9375=CARTESIAN_POINT('Ctrl Pts',(-0.818376780767691,-2.90576385873112,
10.1646415069572));
#9376=CARTESIAN_POINT('Ctrl Pts',(1.97696375273877,-2.2813755899699,10.3219768226283));
#9377=CARTESIAN_POINT('Ctrl Pts',(2.99265430714862,0.396723272524227,10.4793121382995));
#9378=CARTESIAN_POINT('Ctrl Pts',(1.31416190410585,2.71776087645035,10.6366474539706));
#9379=CARTESIAN_POINT('Ctrl Pts',(-1.54714288738549,2.59205032447523,10.7939827696417));
#9380=CARTESIAN_POINT('Ctrl Pts',(-3.01610914676913,0.133199652133039,10.9513180853128));
#9381=CARTESIAN_POINT('Ctrl Pts',(-1.76905884750739,-2.44611374025332,11.108653400984));
#9382=CARTESIAN_POINT('Ctrl Pts',(1.06893599571762,-2.82231343724637,11.2659887166551));
#9383=CARTESIAN_POINT('Ctrl Pts',(2.94774576461505,-0.659848418090555,11.4233240323262));
#9384=CARTESIAN_POINT('Ctrl Pts',(2.1667686505423,2.10078302312668,11.5806593479973));
#9385=CARTESIAN_POINT('Ctrl Pts',(0.35489995180194,2.67388818653474,11.6855495584447));
#9386=CARTESIAN_POINT('Ctrl Pts',(-0.474664453622185,2.51747565713064,11.7379946636685));
#9387=CARTESIAN_POINT('Ctrl Pts',(-1.20564430054384,2.47375567929493,-0.109744663668461));
#9388=CARTESIAN_POINT('Ctrl Pts',(-2.02080199767838,2.07646897882546,-0.0572995584447534));
#9389=CARTESIAN_POINT('Ctrl Pts',(-3.21451394435451,0.420522896515832,0.0475906520026618));
#9390=CARTESIAN_POINT('Ctrl Pts',(-2.11686419183683,-2.45922411196328,0.204925967673786));
#9391=CARTESIAN_POINT('Ctrl Pts',(0.88907666473643,-3.11759018344267,0.362261283344908));
#9392=CARTESIAN_POINT('Ctrl Pts',(3.09329544285396,-0.973179082036162,0.519596599016033));
#9393=CARTESIAN_POINT('Ctrl Pts',(2.51355614196476,2.04925673729017,0.676931914687155));
#9394=CARTESIAN_POINT('Ctrl Pts',(-0.329318085098797,3.22588526469291,0.83426723035828));
#9395=CARTESIAN_POINT('Ctrl Pts',(-2.87553932742704,1.49902076669393,0.991602546029402));
#9396=CARTESIAN_POINT('Ctrl Pts',(-2.8332281113259,-1.57757745247578,1.14893786170053));
#9397=CARTESIAN_POINT('Ctrl Pts',(-0.240320718875223,-3.23385554208785,
1.30627317737165));
#9398=CARTESIAN_POINT('Ctrl Pts',(2.5689019159698,-1.97901104160895,1.46360849304277));
#9399=CARTESIAN_POINT('Ctrl Pts',(3.06554855378139,1.05742886775122,1.6209438087139));
#9400=CARTESIAN_POINT('Ctrl Pts',(0.802503409052275,3.14192384752506,1.77827912438502));
#9401=CARTESIAN_POINT('Ctrl Pts',(-2.18297163768331,2.39799046094296,1.93561444005614));
#9402=CARTESIAN_POINT('Ctrl Pts',(-3.20328253050495,-0.504680192100957,
2.09294975572727));
#9403=CARTESIAN_POINT('Ctrl Pts',(-1.33991649070671,-2.95302201867555,2.25028507139839));
#9404=CARTESIAN_POINT('Ctrl Pts',(1.72967565932795,-2.74298037744955,2.40762038706951));
#9405=CARTESIAN_POINT('Ctrl Pts',(3.24217038064216,-0.0636376955646108,
2.56495570274064));
#9406=CARTESIAN_POINT('Ctrl Pts',(1.83598126768827,2.67299282285076,2.72229101841176));
#9407=CARTESIAN_POINT('Ctrl Pts',(-1.22300448224015,3.00332789927011,2.87962633408289));
#9408=CARTESIAN_POINT('Ctrl Pts',(-3.18101074397215,0.629991214776759,3.036961649754));
#9409=CARTESIAN_POINT('Ctrl Pts',(-2.27539075347452,-2.31047941530565,3.19429696542514));
#9410=CARTESIAN_POINT('Ctrl Pts',(0.678593462518484,-3.1709981403411,3.35163228109625));
#9411=CARTESIAN_POINT('Ctrl Pts',(3.02169070700682,-1.1769042173097,3.50896759676738));
#9412=CARTESIAN_POINT('Ctrl Pts',(2.64458564016939,1.87666860432035,3.6663029124385));
#9413=CARTESIAN_POINT('Ctrl Pts',(-0.113242225622608,3.24081694462443,3.82363822810962));
#9414=CARTESIAN_POINT('Ctrl Pts',(-2.76912658005537,1.68749999972651,3.98097354378075));
#9415=CARTESIAN_POINT('Ctrl Pts',(-2.93217323320329,-1.38494707318046,4.13830885945187));
#9416=CARTESIAN_POINT('Ctrl Pts',(-0.45560346971757,-3.21062980503151,4.295644175123));
#9417=CARTESIAN_POINT('Ctrl Pts',(2.43111204675198,-2.14602247936414,4.45297949079412));
#9418=CARTESIAN_POINT('Ctrl Pts',(3.12927908410086,0.850488494707743,4.61031480646524));
#9419=CARTESIAN_POINT('Ctrl Pts',(1.01039003836266,3.08136824096022,4.76765012213636));
#9420=CARTESIAN_POINT('Ctrl Pts',(-2.01807764432454,2.53832245535854,4.92498543780749));
#9421=CARTESIAN_POINT('Ctrl Pts',(-3.22982085105565,-0.289785327442726,
5.08232075347861));
#9422=CARTESIAN_POINT('Ctrl Pts',(-1.53399773617946,-2.85702103795818,5.23965606914974));
#9423=CARTESIAN_POINT('Ctrl Pts',(1.5427688925436,-2.85229423624577,5.39699138482085));
#9424=CARTESIAN_POINT('Ctrl Pts',(3.23069599088573,-0.279860108625777,5.55432670049199));
#9425=CARTESIAN_POINT('Ctrl Pts',(2.01026894463356,2.54451115858618,5.7116620161631));
#9426=CARTESIAN_POINT('Ctrl Pts',(-1.019852988841,3.07824920158788,5.86899733183423));
#9427=CARTESIAN_POINT('Ctrl Pts',(-3.13187749831153,0.840869550820803,6.02633264750535));
#9428=CARTESIAN_POINT('Ctrl Pts',(-2.42450676654705,-2.15348211157947,6.18366796317648));
#9429=CARTESIAN_POINT('Ctrl Pts',(0.465466204169338,-3.20921477603124,6.3410032788476));
#9430=CARTESIAN_POINT('Ctrl Pts',(2.93641473932339,-1.3759312281592,6.49833859451872));
#9431=CARTESIAN_POINT('Ctrl Pts',(2.76392854664371,1.69600036997724,6.65567391018985));
#9432=CARTESIAN_POINT('Ctrl Pts',(0.103284054131762,3.24114959081836,6.81300922586097));
#9433=CARTESIAN_POINT('Ctrl Pts',(-2.65033935308621,1.86853407234211,6.97034454153209));
#9434=CARTESIAN_POINT('Ctrl Pts',(-3.01806032193904,-1.18618302085242,7.12767985720322));
#9435=CARTESIAN_POINT('Ctrl Pts',(-0.668847147051728,-3.17306819335475,
7.28501517287434));
#9436=CARTESIAN_POINT('Ctrl Pts',(2.28247912613591,-2.30347722049279,7.44235048854546));
#9437=CARTESIAN_POINT('Ctrl Pts',(3.17906002985769,0.639762136724403,7.59968580421659));
#9438=CARTESIAN_POINT('Ctrl Pts',(1.2137707861033,3.00707145645863,7.75702111988771));
#9439=CARTESIAN_POINT('Ctrl Pts',(-1.84418558259193,2.66733908740319,7.91435643555884));
#9440=CARTESIAN_POINT('Ctrl Pts',(-3.24195950004891,-0.0735993116437874,
8.07169175122995));
#9441=CARTESIAN_POINT('Ctrl Pts',(-1.7212395814613,-2.74828174842822,8.22902706690109));
#9442=CARTESIAN_POINT('Ctrl Pts',(1.34898369790163,-2.94889153347749,8.38636238257219));
#9443=CARTESIAN_POINT('Ctrl Pts',(3.20481775972981,-0.494834655687006,8.54369769824334));
#9444=CARTESIAN_POINT('Ctrl Pts',(2.17559394260342,2.40468486103055,8.70103301391445));
#9445=CARTESIAN_POINT('Ctrl Pts',(-0.812154555303452,3.13944635444111,8.85836832958556));
#9446=CARTESIAN_POINT('Ctrl Pts',(-3.06878090276754,1.04799886313063,9.01570364525671));
#9447=CARTESIAN_POINT('Ctrl Pts',(-2.56281335551741,-1.98688354922771,9.17303896092782));
#9448=CARTESIAN_POINT('Ctrl Pts',(0.250263893160364,-3.23312344665729,9.33037427659894));
#9449=CARTESIAN_POINT('Ctrl Pts',(2.83804654185209,-1.56882346716636,9.48770959227006));
#9450=CARTESIAN_POINT('Ctrl Pts',(2.87094937805915,1.50777012013074,9.64504490794121));
#9451=CARTESIAN_POINT('Ctrl Pts',(0.31934842167733,3.22703269386527,9.8023802236123));
#9452=CARTESIAN_POINT('Ctrl Pts',(-2.5197330096178,2.04123559282842,9.95971553928346));
#9453=CARTESIAN_POINT('Ctrl Pts',(-3.09049677227496,-0.982127001208522,
10.1170508549545));
#9454=CARTESIAN_POINT('Ctrl Pts',(-0.879098836487281,-3.1213662060659,10.2743861706257));
#9455=CARTESIAN_POINT('Ctrl Pts',(2.12365083620754,-2.45064947328008,10.4317214862968));
#9456=CARTESIAN_POINT('Ctrl Pts',(3.2147037663447,0.426159411507612,10.5890568019679));
#9457=CARTESIAN_POINT('Ctrl Pts',(1.41167030639802,2.9194137474146,10.7463921176391));
#9458=CARTESIAN_POINT('Ctrl Pts',(-1.66193805120456,2.78437570311449,10.9037274333102));
#9459=CARTESIAN_POINT('Ctrl Pts',(-3.23989891203425,0.143082821950096,11.0610627489813));
#9460=CARTESIAN_POINT('Ctrl Pts',(-1.90031976843527,-2.627610892082,11.2183980646524));
#9461=CARTESIAN_POINT('Ctrl Pts',(1.1482490855046,-3.0317239164071,11.3757333803236));
#9462=CARTESIAN_POINT('Ctrl Pts',(3.16646309234541,-0.708807960139384,11.5330686959947));
#9463=CARTESIAN_POINT('Ctrl Pts',(2.32753890920755,2.25665726929647,11.6904040116658));
#9464=CARTESIAN_POINT('Ctrl Pts',(0.381232877117816,2.87228578439713,11.7952942221132));
#9465=CARTESIAN_POINT('Ctrl Pts',(-0.50988368525031,2.70426773226937,11.8477393273369));
#9466=CARTESIAN_POINT('Ctrl Pts',(-1.28892185405322,2.64462557919718,0.));
#9467=CARTESIAN_POINT('Ctrl Pts',(-2.16038499609476,2.21989706654315,0.0524451052237078));
#9468=CARTESIAN_POINT('Ctrl Pts',(-3.43655029196293,0.449569704103062,0.157335315671123));
#9469=CARTESIAN_POINT('Ctrl Pts',(-2.26308250094201,-2.62909027189387,0.314670631342247));
#9470=CARTESIAN_POINT('Ctrl Pts',(0.950487919687924,-3.33293170930141,0.47200594701337));
#9471=CARTESIAN_POINT('Ctrl Pts',(3.30695885638846,-1.04039954916892,0.629341262684495));
#9472=CARTESIAN_POINT('Ctrl Pts',(2.68717518202235,2.19080519193567,0.786676578355616));
#9473=CARTESIAN_POINT('Ctrl Pts',(-0.352065096336719,3.44870706431028,0.944011894026741));
#9474=CARTESIAN_POINT('Ctrl Pts',(-3.0741616574958,1.60256273346949,1.10134720969786));
#9475=CARTESIAN_POINT('Ctrl Pts',(-3.02892787579111,-1.68654557072963,1.25868252536899));
#9476=CARTESIAN_POINT('Ctrl Pts',(-0.256920408780888,-3.45722787323591,
1.41601784104011));
#9477=CARTESIAN_POINT('Ctrl Pts',(2.74634385856517,-2.11570741037952,1.57335315671124));
#9478=CARTESIAN_POINT('Ctrl Pts',(3.27729540449682,1.13046872625408,1.73068847238236));
#9479=CARTESIAN_POINT('Ctrl Pts',(0.857934783429182,3.35894617427322,1.88802378805348));
#9480=CARTESIAN_POINT('Ctrl Pts',(-2.33375619104173,2.56362702459287,2.0453591037246));
#9481=CARTESIAN_POINT('Ctrl Pts',(-3.42454308987515,-0.539540002481048,
2.20269441939573));
#9482=CARTESIAN_POINT('Ctrl Pts',(-1.43246863664446,-3.15699631612275,2.36002973506685));
#9483=CARTESIAN_POINT('Ctrl Pts',(1.84914966771382,-2.93244645384971,2.51736505073797));
#9484=CARTESIAN_POINT('Ctrl Pts',(3.46611704321809,-0.0680333465830936,
2.6747003664091));
#9485=CARTESIAN_POINT('Ctrl Pts',(1.96279813083206,2.85762464397308,2.83203568208022));
#9486=CARTESIAN_POINT('Ctrl Pts',(-1.30748115679998,3.21077697834334,2.98937099775135));
#9487=CARTESIAN_POINT('Ctrl Pts',(-3.40073292266579,0.673506642233569,3.14670631342246));
#9488=CARTESIAN_POINT('Ctrl Pts',(-2.43255897891363,-2.47007132234958,3.3040416290936));
#9489=CARTESIAN_POINT('Ctrl Pts',(0.725465996449509,-3.39002871776042,3.46137694476471));
#9490=CARTESIAN_POINT('Ctrl Pts',(3.23040816158946,-1.2581966050299,3.61871226043584));
#9491=CARTESIAN_POINT('Ctrl Pts',(2.8272552899658,2.00629586672699,3.77604757610696));
#9492=CARTESIAN_POINT('Ctrl Pts',(-0.12106421383218,3.46467012121918,3.93338289177809));
#9493=CARTESIAN_POINT('Ctrl Pts',(-2.96039865494578,1.80406080581246,4.09071820744921));
#9494=CARTESIAN_POINT('Ctrl Pts',(-3.13470744102623,-1.48060961970634,4.24805352312033));
#9495=CARTESIAN_POINT('Ctrl Pts',(-0.48707340020318,-3.43239786321147,4.40538883879146));
#9496=CARTESIAN_POINT('Ctrl Pts',(2.59903642002639,-2.29425484091306,4.56272415446258));
#9497=CARTESIAN_POINT('Ctrl Pts',(3.3454279982163,0.909234346278705,4.7200594701337));
#9498=CARTESIAN_POINT('Ctrl Pts',(1.0801807804971,3.29420780604002,4.87739478580482));
#9499=CARTESIAN_POINT('Ctrl Pts',(-2.15747246329023,2.71365218072187,5.03473010147595));
#9500=CARTESIAN_POINT('Ctrl Pts',(-3.45291449370647,-0.309801689732533,
5.19206541714708));
#9501=CARTESIAN_POINT('Ctrl Pts',(-1.63995566962662,-3.05436425291692,5.34940073281819));
#9502=CARTESIAN_POINT('Ctrl Pts',(1.64933267669075,-3.04931095649762,5.50673604848933));
#9503=CARTESIAN_POINT('Ctrl Pts',(3.45385008213154,-0.299190905578683,5.66407136416044));
#9504=CARTESIAN_POINT('Ctrl Pts',(2.14912439273668,2.7202683566825,5.82140667983157));
#9505=CARTESIAN_POINT('Ctrl Pts',(-1.0902973660189,3.2908733250419,5.97874199550268));
#9506=CARTESIAN_POINT('Ctrl Pts',(-3.34820589287437,0.898950992404627,6.13607731117382));
#9507=CARTESIAN_POINT('Ctrl Pts',(-2.59197489283764,-2.30222973282867,6.29341262684493));
#9508=CARTESIAN_POINT('Ctrl Pts',(0.497617384004899,-3.43088509381362,6.45074794251607));
#9509=CARTESIAN_POINT('Ctrl Pts',(3.13924192099666,-1.47097102258828,6.60808325818718));
#9510=CARTESIAN_POINT('Ctrl Pts',(2.95484157740695,1.81314832273494,6.76541857385831));
#9511=CARTESIAN_POINT('Ctrl Pts',(0.110418200862072,3.46502574430704,6.92275388952943));
#9512=CARTESIAN_POINT('Ctrl Pts',(-2.8334064294993,1.9975994576497,7.08008920520056));
#9513=CARTESIAN_POINT('Ctrl Pts',(-3.22652701467874,-1.26811632402185,7.23742452087168));
#9514=CARTESIAN_POINT('Ctrl Pts',(-0.715046473049532,-3.39224175569136,
7.3947598365428));
#9515=CARTESIAN_POINT('Ctrl Pts',(2.44013696723805,-2.46258546444229,7.55209515221393));
#9516=CARTESIAN_POINT('Ctrl Pts',(3.39864746673821,0.683952471759619,7.70943046788505));
#9517=CARTESIAN_POINT('Ctrl Pts',(1.29760966092091,3.21477911452065,7.86676578355617));
#9518=CARTESIAN_POINT('Ctrl Pts',(-1.97156914295567,2.85158038765959,8.0241010992273));
#9519=CARTESIAN_POINT('Ctrl Pts',(-3.4658915964548,-0.0786830420698247,
8.18143641489842));
#9520=CARTESIAN_POINT('Ctrl Pts',(-1.84013088404779,-2.93811400679859,8.33877173056954));
#9521=CARTESIAN_POINT('Ctrl Pts',(1.44216214367922,-3.1525805256303,8.49610704624066));
#9522=CARTESIAN_POINT('Ctrl Pts',(3.42618436209615,-0.529014404638419,8.6534423619118));
#9523=CARTESIAN_POINT('Ctrl Pts',(2.32586889591107,2.57078382744821,8.81077767758291));
#9524=CARTESIAN_POINT('Ctrl Pts',(-0.868252563983666,3.35629755313536,8.96811299325404));
#9525=CARTESIAN_POINT('Ctrl Pts',(-3.28075102175166,1.12038736226158,9.12544830892515));
#9526=CARTESIAN_POINT('Ctrl Pts',(-2.73983474254873,-2.12412369627032,9.28278362459629));
#9527=CARTESIAN_POINT('Ctrl Pts',(0.267550388642249,-3.45644520972622,9.44011894026741));
#9528=CARTESIAN_POINT('Ctrl Pts',(3.03407913010768,-1.67718692077769,9.59745425593853));
#9529=CARTESIAN_POINT('Ctrl Pts',(3.06925466623264,1.61191643161116,9.75478957160966));
#9530=CARTESIAN_POINT('Ctrl Pts',(0.341406797653059,3.4499337499385,9.91212488728077));
#9531=CARTESIAN_POINT('Ctrl Pts',(-2.69377870488891,2.18223000239878,10.0694602029519));
#9532=CARTESIAN_POINT('Ctrl Pts',(-3.30396687303986,-1.04996552859114,10.226795518623));
#9533=CARTESIAN_POINT('Ctrl Pts',(-0.939820892206868,-3.33696855340067,
10.3841308342941));
#9534=CARTESIAN_POINT('Ctrl Pts',(2.2703379196763,-2.61992335659027,10.5414661499653));
#9535=CARTESIAN_POINT('Ctrl Pts',(3.43675322554079,0.455595550491001,10.6988014656364));
#9536=CARTESIAN_POINT('Ctrl Pts',(1.50917870869019,3.12106661837885,10.8561367813075));
#9537=CARTESIAN_POINT('Ctrl Pts',(-1.77673321502363,2.97670108175376,11.0134720969786));
#9538=CARTESIAN_POINT('Ctrl Pts',(-3.46368867729937,0.152965991767152,11.1708074126498));
#9539=CARTESIAN_POINT('Ctrl Pts',(-2.03158068936315,-2.80910804391069,11.3281427283209));
#9540=CARTESIAN_POINT('Ctrl Pts',(1.22756217529158,-3.24113439556783,11.485478043992));
#9541=CARTESIAN_POINT('Ctrl Pts',(3.38518042007578,-0.757767502188211,11.6428133596631));
#9542=CARTESIAN_POINT('Ctrl Pts',(2.48830916787281,2.41253151546626,11.8001486753343));
#9543=CARTESIAN_POINT('Ctrl Pts',(0.407565802433691,3.07068338225952,11.9050388857817));
#9544=CARTESIAN_POINT('Ctrl Pts',(-0.545102916878434,2.89105980740811,11.9574839910054));
#9545=CARTESIAN_POINT('Ctrl Pts',(-2.93989309841074,-0.00232834448912937,
10.1778238829104));
#9546=CARTESIAN_POINT('Ctrl Pts',(-2.94219554736775,-0.304542880453153,
10.1941477614813));
#9547=CARTESIAN_POINT('Ctrl Pts',(-2.89923296915434,-0.606119063222061,
10.2104716400522));
#9548=CARTESIAN_POINT('Ctrl Pts',(-2.80824451487588,-0.892433444227729,
10.226795518623));
#9549=CARTESIAN_POINT('Ctrl Pts',(-2.5159182127622,-1.81229987019432,10.2792406238467));
#9550=CARTESIAN_POINT('Ctrl Pts',(-1.72786955248453,-2.5746342117975,10.3316857290704));
#9551=CARTESIAN_POINT('Ctrl Pts',(-0.798818753698492,-2.83629384979735,
10.3841308342941));
#9552=CARTESIAN_POINT('Ctrl Pts',(0.130232045087536,-3.0979534877972,10.4365759395179));
#9553=CARTESIAN_POINT('Ctrl Pts',(1.20028498238192,-2.85893842219374,10.4890210447416));
#9554=CARTESIAN_POINT('Ctrl Pts',(1.92971400200653,-2.22684440487846,10.5414661499653));
#9555=CARTESIAN_POINT('Ctrl Pts',(2.65914302163113,-1.59475038756318,10.593911255189));
#9556=CARTESIAN_POINT('Ctrl Pts',(3.04794812358597,-0.569577418536059,10.6463563604127));
#9557=CARTESIAN_POINT('Ctrl Pts',(2.92108825508827,0.387254243958792,10.6988014656364));
#9558=CARTESIAN_POINT('Ctrl Pts',(2.79422838659058,1.34408590645364,10.7512465708601));
#9559=CARTESIAN_POINT('Ctrl Pts',(2.15170354764038,2.23257626241624,10.8036916760838));
#9560=CARTESIAN_POINT('Ctrl Pts',(1.28278914087964,2.6527605176267,10.8561367813075));
#9561=CARTESIAN_POINT('Ctrl Pts',(0.413874734118906,3.07294477283715,10.9085818865312));
#9562=CARTESIAN_POINT('Ctrl Pts',(-0.681429240452357,3.02482292729546,10.9610269917549));
#9563=CARTESIAN_POINT('Ctrl Pts',(-1.51024047145062,2.53013948952684,11.0134720969786));
#9564=CARTESIAN_POINT('Ctrl Pts',(-1.74480463118476,2.39013776105746,11.0283147313191));
#9565=CARTESIAN_POINT('Ctrl Pts',(-1.95802372783935,2.21436813426865,11.0431573656595));
#9566=CARTESIAN_POINT('Ctrl Pts',(-2.14415473270596,2.01243073062332,11.058));
#9567=CARTESIAN_POINT('Ctrl Pts',(-1.37989654081095,-1.933266887693,1.56125112837913E-17));
#9568=CARTESIAN_POINT('Ctrl Pts',(-1.44414345926609,-1.89839188587405,5.80920822621902E-18));
#9569=CARTESIAN_POINT('Ctrl Pts',(-1.5065284577229,-1.86047032724736,-1.41833741640826E-16));
#9570=CARTESIAN_POINT('Ctrl Pts',(-1.56680444439783,-1.81955553349441,-1.49186218934005E-16));
#9571=CARTESIAN_POINT('Ctrl Pts',(-1.63448180748404,-1.77361675247786,-1.62745475426733E-16));
#9572=CARTESIAN_POINT('Ctrl Pts',(-1.69950176926845,-1.72390575990714,4.47554715783556E-16));
#9573=CARTESIAN_POINT('Ctrl Pts',(-1.76178079551988,-1.6707784873017,5.27355936696949E-16));
#9574=CARTESIAN_POINT('Ctrl Pts',(-1.80277525259689,-1.63580806744237,5.79884178102324E-16));
#9575=CARTESIAN_POINT('Ctrl Pts',(-1.84258178887229,-1.59935636303953,9.13682232518509E-17));
#9576=CARTESIAN_POINT('Ctrl Pts',(-1.88117141744704,-1.56151405921777,1.59594559789866E-16));
#9577=CARTESIAN_POINT('Ctrl Pts',(-1.89157558896771,-1.55131137434519,1.77989100856589E-16));
#9578=CARTESIAN_POINT('Ctrl Pts',(-1.90188938652621,-1.54100934347453,3.40635361961997E-16));
#9579=CARTESIAN_POINT('Ctrl Pts',(-1.91210630257196,-1.53061605927472,3.05311331771918E-16));
#9580=CARTESIAN_POINT('Ctrl Pts',(-1.9724409846318,-1.46923985779222,9.67098202152561E-17));
#9581=CARTESIAN_POINT('Ctrl Pts',(-2.02946085491381,-1.40462521591101,1.4935214824922E-16));
#9582=CARTESIAN_POINT('Ctrl Pts',(-2.08307562783518,-1.33717477526203,1.38777878078145E-16));
#9583=CARTESIAN_POINT('Ctrl Pts',(-2.12998855414138,-1.27815563969417,1.29525391678454E-16));
#9584=CARTESIAN_POINT('Ctrl Pts',(-2.17429437900105,-1.21696417926775,2.01441503266146E-16));
#9585=CARTESIAN_POINT('Ctrl Pts',(-2.21591583956505,-1.15384057343859,1.52655665885959E-16));
#9586=CARTESIAN_POINT('Ctrl Pts',(-2.23664963326987,-1.12239545345888,1.28352927004359E-16));
#9587=CARTESIAN_POINT('Ctrl Pts',(-2.25671701785544,-1.09047047206691,-2.37280165770185E-16));
#9588=CARTESIAN_POINT('Ctrl Pts',(-2.2761066605572,-1.05809323638609,-2.63677968348475E-16));
#9589=CARTESIAN_POINT('Ctrl Pts',(-2.28578146762193,-1.0419380388242,-2.76849621421526E-16));
#9590=CARTESIAN_POINT('Ctrl Pts',(-2.29528887628369,-1.02566760843717,-1.10809144900277E-17));
#9591=CARTESIAN_POINT('Ctrl Pts',(-2.30461525834334,-1.0093071858719,0.));
#9592=CARTESIAN_POINT('Ctrl Pts',(-2.34846766322256,-0.932380906234359,
5.21021705459412E-17));
#9593=CARTESIAN_POINT('Ctrl Pts',(-2.38837887518559,-0.853373340579809,
-1.59588577561705E-17));
#9594=CARTESIAN_POINT('Ctrl Pts',(-2.42425706703596,-0.772682188207588,
-2.77555756156289E-17));
#9595=CARTESIAN_POINT('Ctrl Pts',(-2.46075963346513,-0.690586798283878,
-3.97575872863117E-17));
#9596=CARTESIAN_POINT('Ctrl Pts',(-2.49308822244858,-0.606748001409621,
2.24945356107799E-18));
#9597=CARTESIAN_POINT('Ctrl Pts',(-2.52111243497218,-0.521542915861604,
-2.77555756156289E-17));
#9598=CARTESIAN_POINT('Ctrl Pts',(-2.54406484395513,-0.4517581906252,-5.23303143573299E-17));
#9599=CARTESIAN_POINT('Ctrl Pts',(-2.56412941494483,-0.381055975787894,
-5.2234519399031E-17));
#9600=CARTESIAN_POINT('Ctrl Pts',(-2.58121358727312,-0.309628512371508,
-5.55111512312578E-17));
#9601=CARTESIAN_POINT('Ctrl Pts',(-2.59402671651933,-0.256057914809218,
-5.79686251054279E-17));
#9602=CARTESIAN_POINT('Ctrl Pts',(-2.6051630020304,-0.202079063721199,-1.68485553630616E-16));
#9603=CARTESIAN_POINT('Ctrl Pts',(-2.61457527537642,-0.147769877191515,
-1.94289029309402E-16));
#9604=CARTESIAN_POINT('Ctrl Pts',(-2.617136534184,-0.132991313371873,-2.01310646395843E-16));
#9605=CARTESIAN_POINT('Ctrl Pts',(-2.6195700893165,-0.118188277474481,-3.31395093795537E-16));
#9606=CARTESIAN_POINT('Ctrl Pts',(-2.6218748923051,-0.103362317982878,-3.33066907387547E-16));
#9607=CARTESIAN_POINT('Ctrl Pts',(-2.62397146608191,-0.089875821288789,
-3.34587679685255E-16));
#9608=CARTESIAN_POINT('Ctrl Pts',(-2.62596008221826,-0.076379405564125,
-2.78772373994456E-16));
#9609=CARTESIAN_POINT('Ctrl Pts',(-2.62784009463941,-0.0628763941457686,
-2.77555756156289E-16));
#9610=CARTESIAN_POINT('Ctrl Pts',(-2.64060982150785,0.0288409614284714,
-2.69292046128659E-16));
#9611=CARTESIAN_POINT('Ctrl Pts',(-2.64837710873961,0.12089024959815,-1.76997536955934E-16));
#9612=CARTESIAN_POINT('Ctrl Pts',(-2.65101366112809,0.212875307143708,-1.38777878078145E-16));
#9613=CARTESIAN_POINT('Ctrl Pts',(-2.65226659852151,0.256588270610049,-1.20615204739669E-16));
#9614=CARTESIAN_POINT('Ctrl Pts',(-2.65236023741492,0.300287183221066,-4.34987190636111E-16));
#9615=CARTESIAN_POINT('Ctrl Pts',(-2.6512772014093,0.343931535522003,-4.16333634234434E-16));
#9616=CARTESIAN_POINT('Ctrl Pts',(-2.64907421925761,0.432707650667494,-4.32903459206313E-16));
#9617=CARTESIAN_POINT('Ctrl Pts',(-2.64200629387468,0.521257644934972,-8.62622134822235E-17));
#9618=CARTESIAN_POINT('Ctrl Pts',(-2.63031624428264,0.609320814221094,-8.32667268468867E-17));
#9619=CARTESIAN_POINT('Ctrl Pts',(-2.61839797794639,0.699103179787949,-8.02127613999854E-17));
#9620=CARTESIAN_POINT('Ctrl Pts',(-2.60167524897612,0.788380265268053,1.49019320792917E-16));
#9621=CARTESIAN_POINT('Ctrl Pts',(-2.58035146554209,0.876878238745711,2.4980018054066E-16));
#9622=CARTESIAN_POINT('Ctrl Pts',(-2.57698234718955,0.890860754912604,2.65723370025807E-16));
#9623=CARTESIAN_POINT('Ctrl Pts',(-2.57349826551832,0.904823813068977,1.71128026421916E-16));
#9624=CARTESIAN_POINT('Ctrl Pts',(-2.56989990586492,0.918766319054272,1.94289029309402E-16));
#9625=CARTESIAN_POINT('Ctrl Pts',(-2.56629916621592,0.932718046770052,2.17465351145046E-16));
#9626=CARTESIAN_POINT('Ctrl Pts',(-2.56258611805641,0.946640891227604,-7.03868084514403E-16));
#9627=CARTESIAN_POINT('Ctrl Pts',(-2.55876298044222,0.960529869852388,-6.93889390390723E-16));
#9628=CARTESIAN_POINT('Ctrl Pts',(-2.53419843880054,1.04976976342104,-6.29773977327716E-16));
#9629=CARTESIAN_POINT('Ctrl Pts',(-2.50508011125346,1.13766264916498,6.87890529294335E-17));
#9630=CARTESIAN_POINT('Ctrl Pts',(-2.47169823504828,1.22392740477737,8.32667268468867E-17));
#9631=CARTESIAN_POINT('Ctrl Pts',(-2.43767482619284,1.31184999582573,9.80226325947151E-17));
#9632=CARTESIAN_POINT('Ctrl Pts',(-2.39922225163329,1.39808205966622,-2.50151931196036E-16));
#9633=CARTESIAN_POINT('Ctrl Pts',(-2.35659236008881,1.48232869936419,-2.77555756156289E-16));
#9634=CARTESIAN_POINT('Ctrl Pts',(-2.31360056696885,1.56729054124849,-3.05192222745878E-16));
#9635=CARTESIAN_POINT('Ctrl Pts',(-2.26635993703635,1.65023397727082,5.65740922539343E-17));
#9636=CARTESIAN_POINT('Ctrl Pts',(-2.21507658716517,1.73084671943837,5.55111512312578E-17));
#9637=CARTESIAN_POINT('Ctrl Pts',(-2.18435464293681,1.77913880985734,5.48743828668913E-17));
#9638=CARTESIAN_POINT('Ctrl Pts',(-2.15218088295609,1.82659422289983,-3.64380860772878E-16));
#9639=CARTESIAN_POINT('Ctrl Pts',(-2.11859145320912,1.87314213253736,-3.88578058618805E-16));
#9640=CARTESIAN_POINT('Ctrl Pts',(-2.10923966749503,1.88610174750099,-3.95314910385597E-16));
#9641=CARTESIAN_POINT('Ctrl Pts',(-2.09977706809611,1.89899226435558,-9.16981750261902E-17));
#9642=CARTESIAN_POINT('Ctrl Pts',(-2.0902160744712,1.91179680016256,-1.11022302462516E-16));
#9643=CARTESIAN_POINT('Ctrl Pts',(-2.03140899114824,1.99055403331781,-2.29879778669894E-16));
#9644=CARTESIAN_POINT('Ctrl Pts',(-1.96879105165951,2.06618994280669,4.68887291460301E-17));
#9645=CARTESIAN_POINT('Ctrl Pts',(-1.90263522085423,2.13839704217079,0.));
#9646=CARTESIAN_POINT('Ctrl Pts',(-1.83630675569242,2.21079256674222,-4.70110857922477E-17));
#9647=CARTESIAN_POINT('Ctrl Pts',(-1.76642150904269,2.27974226115238,-1.93865480317173E-16));
#9648=CARTESIAN_POINT('Ctrl Pts',(-1.6932045763485,2.34492041918897,-1.66533453693773E-16));
#9649=CARTESIAN_POINT('Ctrl Pts',(-1.62138195170811,2.40885735573024,-1.39721925040515E-16));
#9650=CARTESIAN_POINT('Ctrl Pts',(-1.54635279514513,2.46916580377976,-2.38947154895597E-16));
#9651=CARTESIAN_POINT('Ctrl Pts',(-1.46828869930752,2.52551090354043,-2.77555756156289E-16));
#9652=CARTESIAN_POINT('Ctrl Pts',(-1.41016377964657,2.56746430557163,-3.06302926317174E-16));
#9653=CARTESIAN_POINT('Ctrl Pts',(-1.35035542782446,2.60721994910279,8.78385754915914E-18));
#9654=CARTESIAN_POINT('Ctrl Pts',(-1.28892185405322,2.64462557919718,0.));
#9655=CARTESIAN_POINT('Origin',(0.,0.,0.));
#9656=CARTESIAN_POINT('Origin',(-1.44337567297407,-2.5,-6.));
#9657=CARTESIAN_POINT('',(-1.44337567297407,-2.5,-6.));
#9658=CARTESIAN_POINT('',(1.44337567297406,-2.5,-6.));
#9659=CARTESIAN_POINT('',(-0.721687836487033,-2.5,-6.));
#9660=CARTESIAN_POINT('',(-1.44337567297407,-2.5,-3.));
#9661=CARTESIAN_POINT('',(-1.44337567297407,-2.5,-6.));
#9662=CARTESIAN_POINT('',(1.44337567297406,-2.5,-3.));
#9663=CARTESIAN_POINT('',(-1.44337567297407,-2.5,-3.));
#9664=CARTESIAN_POINT('',(1.44337567297406,-2.5,-6.));
#9665=CARTESIAN_POINT('Origin',(-2.88675134594813,3.53525079574969E-16,
-6.));
#9666=CARTESIAN_POINT('',(-2.88675134594813,3.53525079574969E-16,-6.));
#9667=CARTESIAN_POINT('',(-2.52590742770461,-0.625,-6.));
#9668=CARTESIAN_POINT('',(-2.88675134594813,5.55111512312578E-16,-3.));
#9669=CARTESIAN_POINT('',(-2.88675134594813,3.53525079574969E-16,-6.));
#9670=CARTESIAN_POINT('',(-2.88675134594813,3.53525079574969E-16,-3.));
#9671=CARTESIAN_POINT('Origin',(-1.44337567297406,2.5,-6.));
#9672=CARTESIAN_POINT('',(-1.44337567297406,2.5,-6.));
#9673=CARTESIAN_POINT('',(-1.80421959121758,1.875,-6.));
#9674=CARTESIAN_POINT('',(-1.44337567297406,2.5,-3.));
#9675=CARTESIAN_POINT('',(-1.44337567297406,2.5,-6.));
#9676=CARTESIAN_POINT('',(-1.44337567297406,2.5,-3.));
#9677=CARTESIAN_POINT('Origin',(1.44337567297406,2.5,-6.));
#9678=CARTESIAN_POINT('',(1.44337567297406,2.5,-6.));
#9679=CARTESIAN_POINT('',(0.721687836487033,2.5,-6.));
#9680=CARTESIAN_POINT('',(1.44337567297406,2.5,-3.));
#9681=CARTESIAN_POINT('',(1.44337567297406,2.5,-6.));
#9682=CARTESIAN_POINT('',(1.44337567297406,2.5,-3.));
#9683=CARTESIAN_POINT('Origin',(2.88675134594813,0.,-6.));
#9684=CARTESIAN_POINT('',(2.88675134594813,0.,-6.));
#9685=CARTESIAN_POINT('',(2.52590742770461,0.625,-6.));
#9686=CARTESIAN_POINT('',(2.88675134594813,0.,-3.));
#9687=CARTESIAN_POINT('',(2.88675134594813,0.,-6.));
#9688=CARTESIAN_POINT('',(2.88675134594813,0.,-3.));
#9689=CARTESIAN_POINT('Origin',(1.44337567297406,-2.5,-6.));
#9690=CARTESIAN_POINT('',(1.80421959121758,-1.875,-6.));
#9691=CARTESIAN_POINT('',(1.44337567297406,-2.5,-3.));
#9692=CARTESIAN_POINT('Origin',(0.,0.,-3.));
#9693=CARTESIAN_POINT('Origin',(0.,0.,0.));
#9694=CARTESIAN_POINT('',(-5.,-6.12323399573677E-16,0.));
#9695=CARTESIAN_POINT('Origin',(0.,0.,0.));
#9696=CARTESIAN_POINT('Origin',(0.,0.,-6.));
#9697=CARTESIAN_POINT('',(-5.,-6.12323399573677E-16,-6.));
#9698=CARTESIAN_POINT('',(-5.,-6.12323399573677E-16,-6.));
#9699=CARTESIAN_POINT('Origin',(0.,0.,-6.));
#9700=CARTESIAN_POINT('Origin',(0.,0.,-6.));
#9701=CARTESIAN_POINT('Origin',(0.,0.,12.));
#9702=CARTESIAN_POINT('',(-380.,-280.,20.));
#9703=CARTESIAN_POINT('',(-360.,-280.,40.));
#9704=CARTESIAN_POINT('',(-380.,280.,20.));
#9705=CARTESIAN_POINT('',(380.,-280.,20.));
#9706=CARTESIAN_POINT('',(380.,280.,20.));
#9707=CARTESIAN_POINT('',(-380.,-260.,40.));
#9708=CARTESIAN_POINT('',(-360.,280.,40.));
#9709=CARTESIAN_POINT('',(-360.,-280.,1000.));
#9710=CARTESIAN_POINT('',(-360.,280.,1000.));
#9711=CARTESIAN_POINT('',(-360.,-180.,520.));
#9712=CARTESIAN_POINT('',(-360.,180.,520.));
#9713=CARTESIAN_POINT('',(-360.,-230.,980.));
#9714=CARTESIAN_POINT('',(-380.,-260.,1000.));
#9715=CARTESIAN_POINT('',(380.,-260.,40.));
#9716=CARTESIAN_POINT('',(380.,-260.,1000.));
#9717=CARTESIAN_POINT('',(0.,0.,61.));
#9718=CARTESIAN_POINT('',(-380.,-280.,10.));
#9719=CARTESIAN_POINT('',(-380.,-280.,0.));
#9720=CARTESIAN_POINT('',(-380.,-280.,1020.));
#9721=CARTESIAN_POINT('',(-400.,300.,1020.));
#9722=CARTESIAN_POINT('',(-300.,-280.,52.));
#9723=CARTESIAN_POINT('',(-300.,-280.,65.));
#9724=CARTESIAN_POINT('',(-360.,170.,980.));
#9725=CARTESIAN_POINT('',(0.,0.,541.));
#9726=CARTESIAN_POINT('',(-380.,280.,10.));
#9727=CARTESIAN_POINT('',(380.,-280.,10.));
#9728=CARTESIAN_POINT('',(380.,280.,10.));
#9729=CARTESIAN_POINT('',(-380.,280.,0.));
#9730=CARTESIAN_POINT('',(380.,-280.,0.));
#9731=CARTESIAN_POINT('',(380.,280.,0.));
#9732=CARTESIAN_POINT('',(-380.,280.,1020.));
#9733=CARTESIAN_POINT('',(380.,-280.,1020.));
#9734=CARTESIAN_POINT('',(380.,280.,1020.));
#9735=CARTESIAN_POINT('',(400.,306.,1020.));
#9736=CARTESIAN_POINT('',(-400.,306.,20.));
#9737=CARTESIAN_POINT('',(400.,300.,20.));
#9738=CARTESIAN_POINT('',(-300.,280.,52.));
#9739=CARTESIAN_POINT('',(300.,-280.,52.));
#9740=CARTESIAN_POINT('',(300.,280.,52.));
#9741=CARTESIAN_POINT('',(-300.,-180.,532.));
#9742=CARTESIAN_POINT('',(-300.,180.,532.));
#9743=CARTESIAN_POINT('',(300.,-180.,532.));
#9744=CARTESIAN_POINT('',(300.,180.,532.));
#9745=CARTESIAN_POINT('',(-300.,280.,65.));
#9746=CARTESIAN_POINT('',(300.,-280.,65.));
#9747=CARTESIAN_POINT('',(300.,280.,65.));
#9748=CARTESIAN_POINT('',(-300.,-180.,545.));
#9749=CARTESIAN_POINT('',(-300.,180.,545.));
#9750=CARTESIAN_POINT('',(300.,-180.,545.));
#9751=CARTESIAN_POINT('',(300.,180.,545.));
#9752=UNCERTAINTY_MEASURE_WITH_UNIT(LENGTH_MEASURE(0.01),#9778,
'DISTANCE_ACCURACY_VALUE',
'Maximum model space distance between geometric entities at asserted c
onnectivities');
#9753=UNCERTAINTY_MEASURE_WITH_UNIT(LENGTH_MEASURE(0.01),#9778,
'DISTANCE_ACCURACY_VALUE',
'Maximum model space distance between geometric entities at asserted c
onnectivities');
#9754=UNCERTAINTY_MEASURE_WITH_UNIT(LENGTH_MEASURE(0.01),#9778,
'DISTANCE_ACCURACY_VALUE',
'Maximum model space distance between geometric entities at asserted c
onnectivities');
#9755=UNCERTAINTY_MEASURE_WITH_UNIT(LENGTH_MEASURE(0.01),#9778,
'DISTANCE_ACCURACY_VALUE',
'Maximum model space distance between geometric entities at asserted c
onnectivities');
#9756=UNCERTAINTY_MEASURE_WITH_UNIT(LENGTH_MEASURE(0.01),#9778,
'DISTANCE_ACCURACY_VALUE',
'Maximum model space distance between geometric entities at asserted c
onnectivities');
#9757=UNCERTAINTY_MEASURE_WITH_UNIT(LENGTH_MEASURE(0.01),#9778,
'DISTANCE_ACCURACY_VALUE',
'Maximum model space distance between geometric entities at asserted c
onnectivities');
#9758=UNCERTAINTY_MEASURE_WITH_UNIT(LENGTH_MEASURE(0.01),#9778,
'DISTANCE_ACCURACY_VALUE',
'Maximum model space distance between geometric entities at asserted c
onnectivities');
#9759=UNCERTAINTY_MEASURE_WITH_UNIT(LENGTH_MEASURE(0.01),#9778,
'DISTANCE_ACCURACY_VALUE',
'Maximum model space distance between geometric entities at asserted c
onnectivities');
#9760=UNCERTAINTY_MEASURE_WITH_UNIT(LENGTH_MEASURE(0.01),#9778,
'DISTANCE_ACCURACY_VALUE',
'Maximum model space distance between geometric entities at asserted c
onnectivities');
#9761=UNCERTAINTY_MEASURE_WITH_UNIT(LENGTH_MEASURE(0.01),#9778,
'DISTANCE_ACCURACY_VALUE',
'Maximum model space distance between geometric entities at asserted c
onnectivities');
#9762=UNCERTAINTY_MEASURE_WITH_UNIT(LENGTH_MEASURE(0.01),#9778,
'DISTANCE_ACCURACY_VALUE',
'Maximum model space distance between geometric entities at asserted c
onnectivities');
#9763=UNCERTAINTY_MEASURE_WITH_UNIT(LENGTH_MEASURE(0.01),#9778,
'DISTANCE_ACCURACY_VALUE',
'Maximum model space distance between geometric entities at asserted c
onnectivities');
#9764=UNCERTAINTY_MEASURE_WITH_UNIT(LENGTH_MEASURE(0.01),#9778,
'DISTANCE_ACCURACY_VALUE',
'Maximum model space distance between geometric entities at asserted c
onnectivities');
#9765=(
GEOMETRIC_REPRESENTATION_CONTEXT(3)
GLOBAL_UNCERTAINTY_ASSIGNED_CONTEXT((#9752))
GLOBAL_UNIT_ASSIGNED_CONTEXT((#9778,#9780,#9781))
REPRESENTATION_CONTEXT('','3D')
);
#9766=(
GEOMETRIC_REPRESENTATION_CONTEXT(3)
GLOBAL_UNCERTAINTY_ASSIGNED_CONTEXT((#9753))
GLOBAL_UNIT_ASSIGNED_CONTEXT((#9778,#9780,#9781))
REPRESENTATION_CONTEXT('','3D')
);
#9767=(
GEOMETRIC_REPRESENTATION_CONTEXT(3)
GLOBAL_UNCERTAINTY_ASSIGNED_CONTEXT((#9754))
GLOBAL_UNIT_ASSIGNED_CONTEXT((#9778,#9780,#9781))
REPRESENTATION_CONTEXT('','3D')
);
#9768=(
GEOMETRIC_REPRESENTATION_CONTEXT(3)
GLOBAL_UNCERTAINTY_ASSIGNED_CONTEXT((#9755))
GLOBAL_UNIT_ASSIGNED_CONTEXT((#9778,#9780,#9781))
REPRESENTATION_CONTEXT('','3D')
);
#9769=(
GEOMETRIC_REPRESENTATION_CONTEXT(3)
GLOBAL_UNCERTAINTY_ASSIGNED_CONTEXT((#9756))
GLOBAL_UNIT_ASSIGNED_CONTEXT((#9778,#9780,#9781))
REPRESENTATION_CONTEXT('','3D')
);
#9770=(
GEOMETRIC_REPRESENTATION_CONTEXT(3)
GLOBAL_UNCERTAINTY_ASSIGNED_CONTEXT((#9757))
GLOBAL_UNIT_ASSIGNED_CONTEXT((#9778,#9780,#9781))
REPRESENTATION_CONTEXT('','3D')
);
#9771=(
GEOMETRIC_REPRESENTATION_CONTEXT(3)
GLOBAL_UNCERTAINTY_ASSIGNED_CONTEXT((#9758))
GLOBAL_UNIT_ASSIGNED_CONTEXT((#9778,#9780,#9781))
REPRESENTATION_CONTEXT('','3D')
);
#9772=(
GEOMETRIC_REPRESENTATION_CONTEXT(3)
GLOBAL_UNCERTAINTY_ASSIGNED_CONTEXT((#9759))
GLOBAL_UNIT_ASSIGNED_CONTEXT((#9778,#9780,#9781))
REPRESENTATION_CONTEXT('','3D')
);
#9773=(
GEOMETRIC_REPRESENTATION_CONTEXT(3)
GLOBAL_UNCERTAINTY_ASSIGNED_CONTEXT((#9760))
GLOBAL_UNIT_ASSIGNED_CONTEXT((#9778,#9780,#9781))
REPRESENTATION_CONTEXT('','3D')
);
#9774=(
GEOMETRIC_REPRESENTATION_CONTEXT(3)
GLOBAL_UNCERTAINTY_ASSIGNED_CONTEXT((#9761))
GLOBAL_UNIT_ASSIGNED_CONTEXT((#9778,#9780,#9781))
REPRESENTATION_CONTEXT('','3D')
);
#9775=(
GEOMETRIC_REPRESENTATION_CONTEXT(3)
GLOBAL_UNCERTAINTY_ASSIGNED_CONTEXT((#9762))
GLOBAL_UNIT_ASSIGNED_CONTEXT((#9778,#9780,#9781))
REPRESENTATION_CONTEXT('','3D')
);
#9776=(
GEOMETRIC_REPRESENTATION_CONTEXT(3)
GLOBAL_UNCERTAINTY_ASSIGNED_CONTEXT((#9763))
GLOBAL_UNIT_ASSIGNED_CONTEXT((#9778,#9780,#9781))
REPRESENTATION_CONTEXT('','3D')
);
#9777=(
GEOMETRIC_REPRESENTATION_CONTEXT(3)
GLOBAL_UNCERTAINTY_ASSIGNED_CONTEXT((#9764))
GLOBAL_UNIT_ASSIGNED_CONTEXT((#9778,#9780,#9781))
REPRESENTATION_CONTEXT('','3D')
);
#9778=(
LENGTH_UNIT()
NAMED_UNIT(*)
SI_UNIT(.MILLI.,.METRE.)
);
#9779=(
LENGTH_UNIT()
NAMED_UNIT(*)
SI_UNIT($,.METRE.)
);
#9780=(
NAMED_UNIT(*)
PLANE_ANGLE_UNIT()
SI_UNIT($,.RADIAN.)
);
#9781=(
NAMED_UNIT(*)
SI_UNIT($,.STERADIAN.)
SOLID_ANGLE_UNIT()
);
#9782=SHAPE_DEFINITION_REPRESENTATION(#9794,#9856);
#9783=SHAPE_DEFINITION_REPRESENTATION(#9795,#9857);
#9784=SHAPE_DEFINITION_REPRESENTATION(#9796,#9858);
#9785=SHAPE_DEFINITION_REPRESENTATION(#9797,#9859);
#9786=SHAPE_DEFINITION_REPRESENTATION(#9798,#9860);
#9787=SHAPE_DEFINITION_REPRESENTATION(#9799,#9861);
#9788=SHAPE_DEFINITION_REPRESENTATION(#9800,#9862);
#9789=SHAPE_DEFINITION_REPRESENTATION(#9801,#9863);
#9790=SHAPE_DEFINITION_REPRESENTATION(#9802,#9864);
#9791=SHAPE_DEFINITION_REPRESENTATION(#9803,#9865);
#9792=SHAPE_DEFINITION_REPRESENTATION(#9804,#9866);
#9793=SHAPE_DEFINITION_REPRESENTATION(#9805,#9867);
#9794=PRODUCT_DEFINITION_SHAPE('',$,#9869);
#9795=PRODUCT_DEFINITION_SHAPE('',$,#9870);
#9796=PRODUCT_DEFINITION_SHAPE('',$,#9871);
#9797=PRODUCT_DEFINITION_SHAPE('',$,#9872);
#9798=PRODUCT_DEFINITION_SHAPE('',$,#9873);
#9799=PRODUCT_DEFINITION_SHAPE('',$,#9874);
#9800=PRODUCT_DEFINITION_SHAPE('',$,#9875);
#9801=PRODUCT_DEFINITION_SHAPE('',$,#9876);
#9802=PRODUCT_DEFINITION_SHAPE('',$,#9877);
#9803=PRODUCT_DEFINITION_SHAPE('',$,#9878);
#9804=PRODUCT_DEFINITION_SHAPE('',$,#9879);
#9805=PRODUCT_DEFINITION_SHAPE('',$,#9880);
#9806=PRODUCT_DEFINITION_SHAPE($,$,#161);
#9807=PRODUCT_DEFINITION_SHAPE($,$,#162);
#9808=PRODUCT_DEFINITION_SHAPE($,$,#163);
#9809=PRODUCT_DEFINITION_SHAPE($,$,#164);
#9810=PRODUCT_DEFINITION_SHAPE($,$,#165);
#9811=PRODUCT_DEFINITION_SHAPE($,$,#166);
#9812=PRODUCT_DEFINITION_SHAPE($,$,#167);
#9813=PRODUCT_DEFINITION_SHAPE($,$,#168);
#9814=PRODUCT_DEFINITION_SHAPE($,$,#169);
#9815=PRODUCT_DEFINITION_SHAPE($,$,#170);
#9816=PRODUCT_DEFINITION_SHAPE($,$,#171);
#9817=PRODUCT_DEFINITION_SHAPE($,$,#172);
#9818=PRODUCT_DEFINITION_SHAPE($,$,#173);
#9819=PRODUCT_DEFINITION_SHAPE($,$,#174);
#9820=PRODUCT_DEFINITION_SHAPE($,$,#175);
#9821=PRODUCT_DEFINITION_SHAPE($,$,#176);
#9822=PRODUCT_DEFINITION_SHAPE($,$,#177);
#9823=PRODUCT_DEFINITION_SHAPE($,$,#178);
#9824=PRODUCT_DEFINITION_SHAPE($,$,#179);
#9825=PRODUCT_DEFINITION_SHAPE($,$,#180);
#9826=PRODUCT_DEFINITION_SHAPE($,$,#181);
#9827=PRODUCT_DEFINITION_SHAPE($,$,#182);
#9828=PRODUCT_DEFINITION_SHAPE($,$,#183);
#9829=PRODUCT_DEFINITION_SHAPE($,$,#184);
#9830=PRODUCT_DEFINITION_SHAPE($,$,#185);
#9831=PRODUCT_DEFINITION_SHAPE($,$,#186);
#9832=PRODUCT_DEFINITION_SHAPE($,$,#187);
#9833=PRODUCT_DEFINITION_SHAPE($,$,#188);
#9834=PRODUCT_DEFINITION_SHAPE($,$,#189);
#9835=PRODUCT_DEFINITION_SHAPE($,$,#190);
#9836=PRODUCT_DEFINITION_SHAPE($,$,#191);
#9837=PRODUCT_DEFINITION_SHAPE($,$,#192);
#9838=PRODUCT_DEFINITION_SHAPE($,$,#193);
#9839=PRODUCT_DEFINITION_SHAPE($,$,#194);
#9840=PRODUCT_DEFINITION_SHAPE($,$,#195);
#9841=PRODUCT_DEFINITION_SHAPE($,$,#196);
#9842=PRODUCT_DEFINITION_SHAPE($,$,#197);
#9843=PRODUCT_DEFINITION_SHAPE($,$,#198);
#9844=PRODUCT_DEFINITION_SHAPE($,$,#199);
#9845=PRODUCT_DEFINITION_SHAPE($,$,#200);
#9846=PRODUCT_DEFINITION_SHAPE($,$,#201);
#9847=PRODUCT_DEFINITION_SHAPE($,$,#202);
#9848=PRODUCT_DEFINITION_SHAPE($,$,#203);
#9849=PRODUCT_DEFINITION_SHAPE($,$,#204);
#9850=PRODUCT_DEFINITION_SHAPE($,$,#205);
#9851=PRODUCT_DEFINITION_SHAPE($,$,#206);
#9852=PRODUCT_DEFINITION_SHAPE($,$,#207);
#9853=PRODUCT_DEFINITION_SHAPE($,$,#208);
#9854=PRODUCT_DEFINITION_SHAPE($,$,#209);
#9855=PRODUCT_DEFINITION_SHAPE($,$,#210);
#9856=SHAPE_REPRESENTATION('',(#3973,#4302,#4303,#4304,#4305,#4306,#4307,
#4308,#4309,#4310,#4311,#4312,#4313,#4314,#4315,#4316,#4317,#4318,#4319,
#4320,#4321,#4322,#4323,#4324,#4325,#4326,#4327,#4328,#4329,#4330,#4331,
#4332,#4333,#4334,#4335,#4336,#4337,#4338,#4339,#4340,#4341,#4342,#4343,
#4344,#4345,#4346,#4347,#4348,#4349,#4350,#4351),#9765);
#9857=SHAPE_REPRESENTATION('',(#3974),#9766);
#9858=SHAPE_REPRESENTATION('',(#4009),#9767);
#9859=SHAPE_REPRESENTATION('',(#4050),#9768);
#9860=SHAPE_REPRESENTATION('',(#4085),#9769);
#9861=SHAPE_REPRESENTATION('',(#4126),#9770);
#9862=SHAPE_REPRESENTATION('',(#4165),#9771);
#9863=SHAPE_REPRESENTATION('',(#4184),#9772);
#9864=SHAPE_REPRESENTATION('',(#4203),#9773);
#9865=SHAPE_REPRESENTATION('',(#4210),#9774);
#9866=SHAPE_REPRESENTATION('',(#4216),#9775);
#9867=SHAPE_REPRESENTATION('',(#4258),#9776);
#9868=PRODUCT_DEFINITION_CONTEXT('part definition',#9906,'design');
#9869=PRODUCT_DEFINITION('MAS-634','MAS-634',#9881,#9868);
#9870=PRODUCT_DEFINITION('Frame post','Frame post',#9882,#9868);
#9871=PRODUCT_DEFINITION('Frame rail','Frame rail',#9883,#9868);
#9872=PRODUCT_DEFINITION('End rail','End rail',#9884,#9868);
#9873=PRODUCT_DEFINITION('Equipment mounting channel',
'Equipment mounting channel',#9885,#9868);
#9874=PRODUCT_DEFINITION('Equipment shelf','Equipment shelf',#9886,#9868);
#9875=PRODUCT_DEFINITION('Foot plate','Foot plate',#9887,#9868);
#9876=PRODUCT_DEFINITION('Isolation pad','Isolation pad',#9888,#9868);
#9877=PRODUCT_DEFINITION('Post cap','Post cap',#9889,#9868);
#9878=PRODUCT_DEFINITION('Frame gusset','Frame gusset',#9890,#9868);
#9879=PRODUCT_DEFINITION('Rivet nut M6','Rivet nut M6',#9891,#9868);
#9880=PRODUCT_DEFINITION('Socket head cap screw M6x12',
'Socket head cap screw M6x12',#9892,#9868);
#9881=PRODUCT_DEFINITION_FORMATION('',$,#9908);
#9882=PRODUCT_DEFINITION_FORMATION('',$,#9909);
#9883=PRODUCT_DEFINITION_FORMATION('',$,#9910);
#9884=PRODUCT_DEFINITION_FORMATION('',$,#9911);
#9885=PRODUCT_DEFINITION_FORMATION('',$,#9912);
#9886=PRODUCT_DEFINITION_FORMATION('',$,#9913);
#9887=PRODUCT_DEFINITION_FORMATION('',$,#9914);
#9888=PRODUCT_DEFINITION_FORMATION('',$,#9915);
#9889=PRODUCT_DEFINITION_FORMATION('',$,#9916);
#9890=PRODUCT_DEFINITION_FORMATION('',$,#9917);
#9891=PRODUCT_DEFINITION_FORMATION('',$,#9918);
#9892=PRODUCT_DEFINITION_FORMATION('',$,#9919);
#9893=PRODUCT_RELATED_PRODUCT_CATEGORY('MAS-634','MAS-634',(#9908));
#9894=PRODUCT_RELATED_PRODUCT_CATEGORY('Frame post','Frame post',(#9909));
#9895=PRODUCT_RELATED_PRODUCT_CATEGORY('Frame rail','Frame rail',(#9910));
#9896=PRODUCT_RELATED_PRODUCT_CATEGORY('End rail','End rail',(#9911));
#9897=PRODUCT_RELATED_PRODUCT_CATEGORY('Equipment mounting channel',
'Equipment mounting channel',(#9912));
#9898=PRODUCT_RELATED_PRODUCT_CATEGORY('Equipment shelf',
'Equipment shelf',(#9913));
#9899=PRODUCT_RELATED_PRODUCT_CATEGORY('Foot plate','Foot plate',(#9914));
#9900=PRODUCT_RELATED_PRODUCT_CATEGORY('Isolation pad','Isolation pad',
(#9915));
#9901=PRODUCT_RELATED_PRODUCT_CATEGORY('Post cap','Post cap',(#9916));
#9902=PRODUCT_RELATED_PRODUCT_CATEGORY('Frame gusset','Frame gusset',(#9917));
#9903=PRODUCT_RELATED_PRODUCT_CATEGORY('Rivet nut M6','Rivet nut M6',(#9918));
#9904=PRODUCT_RELATED_PRODUCT_CATEGORY('Socket head cap screw M6x12',
'Socket head cap screw M6x12',(#9919));
#9905=APPLICATION_PROTOCOL_DEFINITION('international standard',
'automotive_design',2009,#9906);
#9906=APPLICATION_CONTEXT(
'Core Data for Automotive Mechanical Design Process');
#9907=PRODUCT_CONTEXT('part definition',#9906,'mechanical');
#9908=PRODUCT('MAS-634','MAS-634',
'Independent AHU equipment rack. Nominal800x600 frame on1000long40squa
re aluminum posts; two removable notched shelves; welded perimeter/cro
ss rails and rear gussets; two mounting channels; four isolation pads 
and anchor-ready feet. Imported native extrusion library retained and 
cut-length parameters customized per family. Shelf hardware uses model
ed M6 rivet nuts and screws. Weld design, floor anchors and load ratin
g require engineering selection.',(#9907));
#9909=PRODUCT('Frame post','Frame post',
'Independent aluminum extrusion section. Whole-mm nominal die dimensio
ns; parametric saw-cut length. Select structural loading, tolerances a
nd finish for the assembly application.',(#9907));
#9910=PRODUCT('Frame rail','Frame rail',
'Independent aluminum extrusion section. Whole-mm nominal die dimensio
ns; parametric saw-cut length. Select structural loading, tolerances a
nd finish for the assembly application.',(#9907));
#9911=PRODUCT('End rail','End rail',
'Independent aluminum extrusion section. Whole-mm nominal die dimensio
ns; parametric saw-cut length. Select structural loading, tolerances a
nd finish for the assembly application.',(#9907));
#9912=PRODUCT('Equipment mounting channel','Equipment mounting channel',

'Independent aluminum extrusion section. Whole-mm nominal die dimensio
ns; parametric saw-cut length. Select structural loading, tolerances a
nd finish for the assembly application.',(#9907));
#9913=PRODUCT('Equipment shelf','Equipment shelf',$,(#9907));
#9914=PRODUCT('Foot plate','Foot plate',$,(#9907));
#9915=PRODUCT('Isolation pad','Isolation pad',$,(#9907));
#9916=PRODUCT('Post cap','Post cap',$,(#9907));
#9917=PRODUCT('Frame gusset','Frame gusset',$,(#9907));
#9918=PRODUCT('Rivet nut M6','Rivet nut M6',$,(#9907));
#9919=PRODUCT('Socket head cap screw M6x12',
'Socket head cap screw M6x12',$,(#9907));
#9920=PRESENTATION_STYLE_ASSIGNMENT((#9931));
#9921=PRESENTATION_STYLE_ASSIGNMENT((#9932));
#9922=PRESENTATION_STYLE_ASSIGNMENT((#9933));
#9923=PRESENTATION_STYLE_ASSIGNMENT((#9934));
#9924=PRESENTATION_STYLE_ASSIGNMENT((#9935));
#9925=PRESENTATION_STYLE_ASSIGNMENT((#9936));
#9926=PRESENTATION_STYLE_ASSIGNMENT((#9937));
#9927=PRESENTATION_STYLE_ASSIGNMENT((#9938));
#9928=PRESENTATION_STYLE_ASSIGNMENT((#9939));
#9929=PRESENTATION_STYLE_ASSIGNMENT((#9940));
#9930=PRESENTATION_STYLE_ASSIGNMENT((#9941));
#9931=SURFACE_STYLE_USAGE(.BOTH.,#9942);
#9932=SURFACE_STYLE_USAGE(.BOTH.,#9943);
#9933=SURFACE_STYLE_USAGE(.BOTH.,#9944);
#9934=SURFACE_STYLE_USAGE(.BOTH.,#9945);
#9935=SURFACE_STYLE_USAGE(.BOTH.,#9946);
#9936=SURFACE_STYLE_USAGE(.BOTH.,#9947);
#9937=SURFACE_STYLE_USAGE(.BOTH.,#9948);
#9938=SURFACE_STYLE_USAGE(.BOTH.,#9949);
#9939=SURFACE_STYLE_USAGE(.BOTH.,#9950);
#9940=SURFACE_STYLE_USAGE(.BOTH.,#9951);
#9941=SURFACE_STYLE_USAGE(.BOTH.,#9952);
#9942=SURFACE_SIDE_STYLE('',(#9953));
#9943=SURFACE_SIDE_STYLE('',(#9954));
#9944=SURFACE_SIDE_STYLE('',(#9955));
#9945=SURFACE_SIDE_STYLE('',(#9956));
#9946=SURFACE_SIDE_STYLE('',(#9957));
#9947=SURFACE_SIDE_STYLE('',(#9958));
#9948=SURFACE_SIDE_STYLE('',(#9959));
#9949=SURFACE_SIDE_STYLE('',(#9960));
#9950=SURFACE_SIDE_STYLE('',(#9961));
#9951=SURFACE_SIDE_STYLE('',(#9962));
#9952=SURFACE_SIDE_STYLE('',(#9963));
#9953=SURFACE_STYLE_FILL_AREA(#9964);
#9954=SURFACE_STYLE_FILL_AREA(#9965);
#9955=SURFACE_STYLE_FILL_AREA(#9966);
#9956=SURFACE_STYLE_FILL_AREA(#9967);
#9957=SURFACE_STYLE_FILL_AREA(#9968);
#9958=SURFACE_STYLE_FILL_AREA(#9969);
#9959=SURFACE_STYLE_FILL_AREA(#9970);
#9960=SURFACE_STYLE_FILL_AREA(#9971);
#9961=SURFACE_STYLE_FILL_AREA(#9972);
#9962=SURFACE_STYLE_FILL_AREA(#9973);
#9963=SURFACE_STYLE_FILL_AREA(#9974);
#9964=FILL_AREA_STYLE('Steel - Satin',(#9975));
#9965=FILL_AREA_STYLE('Frame gray',(#9976));
#9966=FILL_AREA_STYLE('Dark blue',(#9977));
#9967=FILL_AREA_STYLE('Sky blue',(#9978));
#9968=FILL_AREA_STYLE('Light blue',(#9979));
#9969=FILL_AREA_STYLE('Foot gray',(#9980));
#9970=FILL_AREA_STYLE('Pad charcoal',(#9981));
#9971=FILL_AREA_STYLE('Cap gray',(#9982));
#9972=FILL_AREA_STYLE('Gusset gray',(#9983));
#9973=FILL_AREA_STYLE('Nut gray',(#9984));
#9974=FILL_AREA_STYLE('Dark gray',(#9985));
#9975=FILL_AREA_STYLE_COLOUR('Steel - Satin',#9986);
#9976=FILL_AREA_STYLE_COLOUR('Frame gray',#9987);
#9977=FILL_AREA_STYLE_COLOUR('Dark blue',#9988);
#9978=FILL_AREA_STYLE_COLOUR('Sky blue',#9989);
#9979=FILL_AREA_STYLE_COLOUR('Light blue',#9990);
#9980=FILL_AREA_STYLE_COLOUR('Foot gray',#9991);
#9981=FILL_AREA_STYLE_COLOUR('Pad charcoal',#9992);
#9982=FILL_AREA_STYLE_COLOUR('Cap gray',#9993);
#9983=FILL_AREA_STYLE_COLOUR('Gusset gray',#9994);
#9984=FILL_AREA_STYLE_COLOUR('Nut gray',#9995);
#9985=FILL_AREA_STYLE_COLOUR('Dark gray',#9996);
#9986=COLOUR_RGB('Steel - Satin',0.627450980392157,0.627450980392157,0.627450980392157);
#9987=COLOUR_RGB('Frame gray',0.407843137254902,0.447058823529412,0.498039215686275);
#9988=COLOUR_RGB('Dark blue',0.0901960784313725,0.270588235294118,0.513725490196078);
#9989=COLOUR_RGB('Sky blue',0.317647058823529,0.686274509803922,0.890196078431372);
#9990=COLOUR_RGB('Light blue',0.662745098039216,0.831372549019608,0.949019607843137);
#9991=COLOUR_RGB('Foot gray',0.407843137254902,0.447058823529412,0.498039215686275);
#9992=COLOUR_RGB('Pad charcoal',0.164705882352941,0.184313725490196,0.211764705882353);
#9993=COLOUR_RGB('Cap gray',0.725490196078431,0.752941176470588,0.792156862745098);
#9994=COLOUR_RGB('Gusset gray',0.407843137254902,0.447058823529412,0.498039215686275);
#9995=COLOUR_RGB('Nut gray',0.407843137254902,0.447058823529412,0.498039215686275);
#9996=COLOUR_RGB('Dark gray',0.250980392156863,0.282352941176471,0.32156862745098);
ENDSEC;
END-ISO-10303-21;
